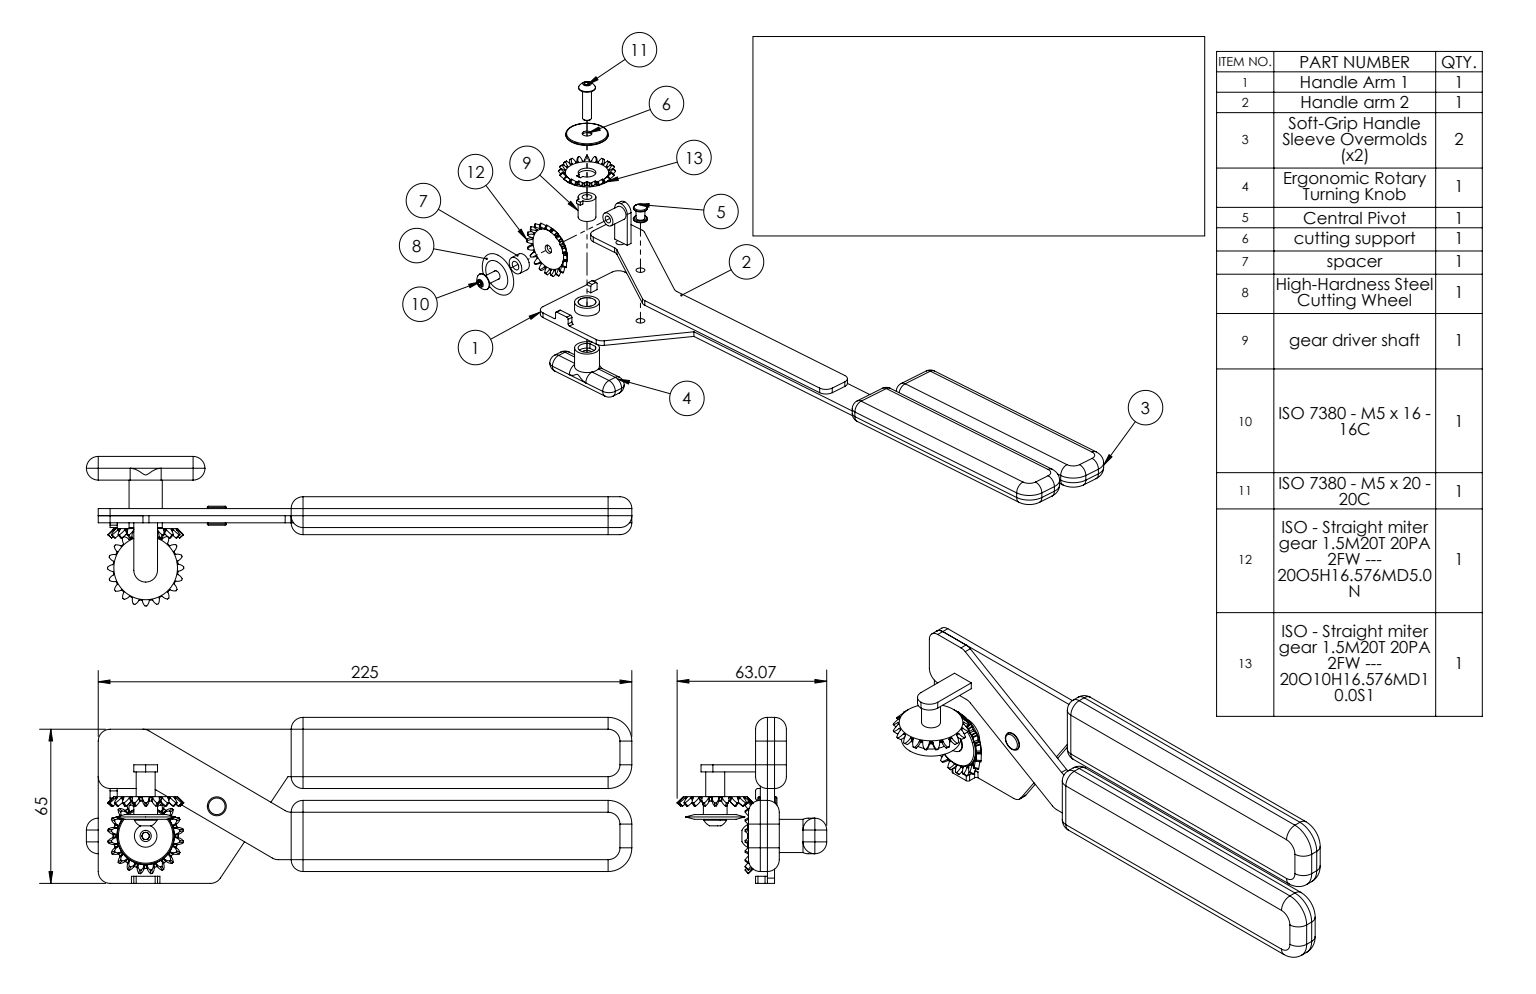
ISO-10303-21;
HEADER;
FILE_DESCRIPTION (('STEP AP214'),
    '1' );
FILE_NAME ('BR-823',
    '2026-09-24T10:15:42',
    ( '' ),
    ( '' ),
    'SwSTEP 2.0',
    'SolidWorks 2026',
    '' );
FILE_SCHEMA (( 'AUTOMOTIVE_DESIGN' ));
ENDSEC;

DATA;
#1 = PRODUCT_DEFINITION_CONTEXT ( 'detailed design', #13776, 'design' ) ;
#2 = DIRECTION ( 'NONE',  ( 0.000000000000000000, 0.000000000000000000, -1.000000000000000000 ) ) ;
#3 = VERTEX_POINT ( 'NONE', #8497 ) ;
#4 = ORIENTED_EDGE ( 'NONE', *, *, #17500, .T. ) ;
#5 = B_SPLINE_CURVE_WITH_KNOTS ( 'NONE', 3,
 ( #7725, #1687, #4752, #9340, #164, #3200, #16319, #9048, #7824, #13639, #557, #15165, #451 ),
 .UNSPECIFIED., .F., .F.,
 ( 4, 3, 3, 3, 4 ),
 ( 1.788933584601082316E-18, 0.0002299804304191483382, 0.0004599608082120253344, 0.0006467586077648016917, 0.0008336169836825988323 ),
 .UNSPECIFIED. ) ;
#6 = CARTESIAN_POINT ( 'NONE',  ( 3.950837973638668288, 0.000000000000000000, 0.000000000000000000 ) ) ;
#8 = ORIENTED_EDGE ( 'NONE', *, *, #17820, .T. ) ;
#7 = CARTESIAN_POINT ( 'NONE',  ( 1.254009781011409919, 5.487405433548389055, 13.61532727684416955 ) ) ;
#9 = CARTESIAN_POINT ( 'NONE',  ( 8.438534575730034959, 3.845978796786118981, -5.688336279099003079 ) ) ;
#10 = DIRECTION ( 'NONE',  ( -0.000000000000000000, 1.000000000000000000, -0.000000000000000000 ) ) ;
#11 = ORIENTED_EDGE ( 'NONE', *, *, #5609, .T. ) ;
#12 = DIRECTION ( 'NONE',  ( -1.000000000000000000, 0.000000000000000000, 0.000000000000000000 ) ) ;
#13 = CARTESIAN_POINT ( 'NONE',  ( 6.538348415311012296, -7.500000000000000888, -12.00000000000000000 ) ) ;
#14 = ORIENTED_EDGE ( 'NONE', *, *, #2662, .F. ) ;
#15 = CARTESIAN_POINT ( 'NONE',  ( 0.3137051932979775248, -0.4596302728638797519, -13.73004976592202553 ) ) ;
#16 =( NAMED_UNIT ( * ) SI_UNIT ( $, .STERADIAN. ) SOLID_ANGLE_UNIT ( ) );
#17 = DIRECTION ( 'NONE',  ( 1.000000000000000000, 0.000000000000000000, 0.000000000000000000 ) ) ;
#18 = CARTESIAN_POINT ( 'NONE',  ( 0.4862570985993235340, -13.89016912371018186, 0.7479633556561964269 ) ) ;
#19 = ADVANCED_FACE ( 'NONE', ( #12879 ), #13081, .T. ) ;
#20 = ADVANCED_FACE ( 'NONE', ( #6722 ), #7157, .F. ) ;
#21 = DIRECTION ( 'NONE',  ( -1.000000000000000000, -0.000000000000000000, -0.000000000000000000 ) ) ;
#22 = CARTESIAN_POINT ( 'NONE',  ( 0.3137051932979775248, 10.83767969834815581, -8.442169467526731808 ) ) ;
#23 =( BOUNDED_SURFACE ( )  B_SPLINE_SURFACE ( 3, 2, ( 
 ( #9096, #13, #15967 ),
 ( #13391, #10337, #14824 ),
 ( #11773, #4513, #14919 ),
 ( #3147, #1737, #16166 ),
 ( #3050, #14723, #10241 ),
 ( #5830, #6041, #1634 ),
 ( #16367, #7585, #7479 ),
 ( #8709, #13293, #11868 ),
 ( #17403, #308, #4405 ),
 ( #11673, #17708, #11585 ),
 ( #4605, #13483, #14634 ),
 ( #10432, #2857, #16066 ),
 ( #10529, #6137, #4319 ),
 ( #1837, #2958, #14535 ),
 ( #11963, #3250, #7675 ),
 ( #1450, #8805, #1543 ),
 ( #7383, #112, #18081 ),
 ( #4980, #16642, #4896 ),
 ( #1935, #13772, #10817 ),
 ( #3545, #6425, #502 ),
 ( #15014, #6332, #12161 ),
 ( #13684, #7870, #13859 ),
 ( #12251, #7768, #685 ),
 ( #777, #6517, #13581 ),
 ( #598, #3730, #9385 ),
 ( #16464, #9186, #5164 ),
 ( #6228, #10723, #12335 ),
 ( #2209, #3349, #8051 ),
 ( #15212, #12061, #18171 ),
 ( #17895, #2122, #17990 ),
 ( #7963, #5070, #3447 ),
 ( #15113, #9558, #10920 ),
 ( #16558, #16740, #4798 ),
 ( #3639, #11009, #16826 ),
 ( #9474, #15389, #9281 ),
 ( #15296, #6610, #2295 ),
 ( #12433, #18262, #8141 ),
 ( #399, #10633, #2029 ),
 ( #867, #11100, #16916 ),
 ( #5524, #4007, #17020 ),
 ( #5350, #5441, #11374 ),
 ( #2657, #12703, #11287 ),
 ( #17193, #15481, #8406 ),
 ( #6984, #18535, #1038 ) ),
 .UNSPECIFIED., .F., .F., .T. ) 
 B_SPLINE_SURFACE_WITH_KNOTS ( ( 4, 2, 2, 2, 2, 2, 2, 2, 2, 2, 2, 2, 2, 2, 2, 2, 2, 2, 2, 2, 2, 4 ),
 ( 3, 3 ),
 ( 0.007984881688765531685, 0.008880023643941203221, 0.009775165599116873022, 0.01067030755429254282, 0.01156544950946821262, 0.01246059146464388243, 0.01335573341981955396, 0.01425087537499522550, 0.01469844635258306040, 0.01492223184137697785, 0.01514601733017089530, 0.01536980281896481275, 0.01559358830775873020, 0.01581737379655264591, 0.01604115928534656510, 0.01693630124052223490, 0.01783144319569790470, 0.01872658515087357797, 0.01962172710604925124, 0.02051686906122492104, 0.02141201101640059085, 0.02230715297157626065 ),
 ( 0.000000000000000000, 1.000000000000000000 ),
 .UNSPECIFIED. ) 
 GEOMETRIC_REPRESENTATION_ITEM ( )  RATIONAL_B_SPLINE_SURFACE ( (
 ( 1.000000000000000000, 0.7071067811865474617, 1.000000000000000000),
 ( 1.000000000000000000, 0.7141735847353027911, 1.000000000000000000),
 ( 1.000000000000000000, 0.7220150969518837059, 1.000000000000000000),
 ( 1.000000000000000000, 0.7390483610380735868, 1.000000000000000000),
 ( 1.000000000000000000, 0.7482852340371979327, 1.000000000000000000),
 ( 1.000000000000000000, 0.7685052920442676516, 1.000000000000000000),
 ( 1.000000000000000000, 0.7795547470752138830, 1.000000000000000000),
 ( 1.000000000000000000, 0.8031735375541008137, 1.000000000000000000),
 ( 1.000000000000000000, 0.8157770400072400507, 1.000000000000000000),
 ( 1.000000000000000000, 0.8424364036431882807, 1.000000000000000000),
 ( 1.000000000000000000, 0.8565278543580017168, 1.000000000000000000),
 ( 1.000000000000000000, 0.8853337094945018526, 1.000000000000000000),
 ( 1.000000000000000000, 0.9000757013528668526, 1.000000000000000000),
 ( 1.000000000000000000, 0.9285356150544983311, 1.000000000000000000),
 ( 1.000000000000000000, 0.9423225300521810288, 1.000000000000000000),
 ( 1.000000000000000000, 0.9592421851076473605, 1.000000000000000000),
 ( 1.000000000000000000, 0.9642414584271679079, 1.000000000000000000),
 ( 1.000000000000000000, 0.9699277023943830844, 1.000000000000000000),
 ( 1.000000000000000000, 0.9715166551480127755, 1.000000000000000000),
 ( 1.000000000000000000, 0.9737696706145027026, 1.000000000000000000),
 ( 1.000000000000000000, 0.9744508395083844032, 1.000000000000000000),
 ( 1.000000000000000000, 0.9748110790397115366, 1.000000000000000000),
 ( 1.000000000000000000, 0.9744748476087098377, 1.000000000000000000),
 ( 1.000000000000000000, 0.9728601655991807595, 1.000000000000000000),
 ( 1.000000000000000000, 0.9715893508620213614, 1.000000000000000000),
 ( 1.000000000000000000, 0.9682746065025299442, 1.000000000000000000),
 ( 1.000000000000000000, 0.9662330922797159882, 1.000000000000000000),
 ( 1.000000000000000000, 0.9616633680012534047, 1.000000000000000000),
 ( 1.000000000000000000, 0.9591230388079813318, 1.000000000000000000),
 ( 1.000000000000000000, 0.9454866025348970249, 1.000000000000000000),
 ( 1.000000000000000000, 0.9317605398179185094, 1.000000000000000000),
 ( 1.000000000000000000, 0.9032287473899394126, 1.000000000000000000),
 ( 1.000000000000000000, 0.8883390392773794497, 1.000000000000000000),
 ( 1.000000000000000000, 0.8592388025803222584, 1.000000000000000000),
 ( 1.000000000000000000, 0.8450030273492604715, 1.000000000000000000),
 ( 1.000000000000000000, 0.8179255325836626289, 1.000000000000000000),
 ( 1.000000000000000000, 0.8050698650503591569, 1.000000000000000000),
 ( 1.000000000000000000, 0.7808988731588855092, 1.000000000000000000),
 ( 1.000000000000000000, 0.7696290231168715357, 1.000000000000000000),
 ( 1.000000000000000000, 0.7490294503509588031, 1.000000000000000000),
 ( 1.000000000000000000, 0.7396188834547082758, 1.000000000000000000),
 ( 1.000000000000000000, 0.7222670797466549386, 1.000000000000000000),
 ( 1.000000000000000000, 0.7142721232192638103, 1.000000000000000000),
 ( 1.000000000000000000, 0.7071067811865517916, 1.000000000000000000) ) ) 
 REPRESENTATION_ITEM ( '' )  SURFACE ( )  );
#24 = FACE_OUTER_BOUND ( 'NONE', #1681, .T. ) ;
#25 = CARTESIAN_POINT ( 'NONE',  ( 0.4862570985993252548, 11.67702470553365401, 7.559321496869467971 ) ) ;
#26 = FACE_BOUND ( 'NONE', #13698, .T. ) ;
#27 = ORIENTED_EDGE ( 'NONE', *, *, #8314, .T. ) ;
#28 = DIRECTION ( 'NONE',  ( 0.000000000000000000, 0.000000000000000000, 1.000000000000000000 ) ) ;
#29 = DIRECTION ( 'NONE',  ( -1.000000000000000000, -0.000000000000000000, -0.000000000000000000 ) ) ;
#30 = ORIENTED_EDGE ( 'NONE', *, *, #17968, .F. ) ;
#31 = VERTEX_POINT ( 'NONE', #18279 ) ;
#33 = CARTESIAN_POINT ( 'NONE',  ( 16.57210152137263393, 0.01136813053532075186, 0.009075239946108242667 ) ) ;
#32 = AXIS2_PLACEMENT_3D ( 'NONE', #18894, #175, #17469 ) ;
#34 = ORIENTED_EDGE ( 'NONE', *, *, #3133, .F. ) ;
#35 = CARTESIAN_POINT ( 'NONE',  ( 0.4862570985993252548, 11.67702470553365401, 7.559321496869467971 ) ) ;
#36 = ORIENTED_EDGE ( 'NONE', *, *, #16394, .F. ) ;
#37 = CARTESIAN_POINT ( 'NONE',  ( 16.56822296793089322, -0.007741272030791128758, 0.006547366384936715959 ) ) ;
#38 = CARTESIAN_POINT ( 'NONE',  ( 0.8740779401507028368, 12.04241618260048696, 7.708543377337672808 ) ) ;
#39 = CARTESIAN_POINT ( 'NONE',  ( -30.00000000000000355, -12.50000000000000178, 6.000000000000000000 ) ) ;
#40 = CARTESIAN_POINT ( 'NONE',  ( 2.747332970342022840, -7.555624153089539163, -14.49942876448600693 ) ) ;
#41 = UNCERTAINTY_MEASURE_WITH_UNIT (LENGTH_MEASURE( 1.000000000000000082E-05 ), #17046, 'distance_accuracy_value', 'NONE');
#42 = PRODUCT_DEFINITION_SHAPE ( 'NONE', 'NONE',  #2847 ) ;
#43 = DIRECTION ( 'NONE',  ( -1.000000000000000000, -0.000000000000000000, -0.000000000000000000 ) ) ;
#44 = DIRECTION ( 'NONE',  ( -0.000000000000000000, 1.000000000000000000, -0.000000000000000000 ) ) ;
#45 =( NAMED_UNIT ( * ) PLANE_ANGLE_UNIT ( ) SI_UNIT ( $, .RADIAN. ) );
#46 = CARTESIAN_POINT ( 'NONE',  ( 3.686287386450715076E-15, -27.00000000000000000, 25.01316734529526187 ) ) ;
#47 = LINE ( 'NONE', #1670, #13971 ) ;
#48 = ADVANCED_FACE ( 'NONE', ( #881 ), #6440, .F. ) ;
#49 = ADVANCED_FACE ( 'NONE', ( #15133 ), #3233, .F. ) ;
#50 = CARTESIAN_POINT ( 'NONE',  ( 16.58200780006414732, 0.01080144354108870768, 0.002844973367391462511 ) ) ;
#51 = CARTESIAN_POINT ( 'NONE',  ( 2.123976203522053297, -14.31368049382965069, -6.261444813538707521 ) ) ;
#52 = EDGE_LOOP ( 'NONE', ( #9471, #1055, #7657, #12818 ) ) ;
#53 = DIRECTION ( 'NONE',  ( 0.000000000000000000, 0.000000000000000000, 1.000000000000000000 ) ) ;
#54 = AXIS2_PLACEMENT_3D ( 'NONE', #4201, #10016, #14696 ) ;
#55 = ORIENTED_EDGE ( 'NONE', *, *, #1230, .F. ) ;
#56 = EDGE_CURVE ( 'NONE', #18903, #4935, #3396, .T. ) ;
#57 = ORIENTED_EDGE ( 'NONE', *, *, #11432, .T. ) ;
#58 = EDGE_LOOP ( 'NONE', ( #12912, #14842, #3064, #3403, #10811, #3564 ) ) ;
#59 = ORIENTED_EDGE ( 'NONE', *, *, #10784, .F. ) ;
#60 = CARTESIAN_POINT ( 'NONE',  ( 1.918921323896324083, -12.08297777410667173, 3.258415356426475729 ) ) ;
#61 = CARTESIAN_POINT ( 'NONE',  ( 1.846138399168762989, -3.446241763653083101, 11.95493567637849530 ) ) ;
#62 =( BOUNDED_SURFACE ( )  B_SPLINE_SURFACE ( 3, 1, ( 
 ( #17504, #8616 ),
 ( #15879, #10145 ),
 ( #4407, #16068 ),
 ( #12913, #2960 ) ),
 .UNSPECIFIED., .F., .F., .T. ) 
 B_SPLINE_SURFACE_WITH_KNOTS ( ( 4, 4 ),
 ( 2, 2 ),
 ( 0.000000000000000000, 1.000000000000000000 ),
 ( 0.000000000000000000, 1.000000000000000000 ),
 .UNSPECIFIED. ) 
 GEOMETRIC_REPRESENTATION_ITEM ( )  RATIONAL_B_SPLINE_SURFACE ( (
 ( 1.000000000000000000, 1.000000000000000000),
 ( 0.9933953342250436691, 0.8357391271907733676),
 ( 0.9933953342250436691, 0.8357391271907733676),
 ( 1.000000000000000000, 1.000000000000000000) ) ) 
 REPRESENTATION_ITEM ( '' )  SURFACE ( )  );
#63 = CARTESIAN_POINT ( 'NONE',  ( 0.3151926232592472954, 8.013596737356548871, -11.16039997398644879 ) ) ;
#64 = ORIENTED_EDGE ( 'NONE', *, *, #16293, .T. ) ;
#65 = CARTESIAN_POINT ( 'NONE',  ( -110.4113270445337918, -81.60345299795268659, -91.28051051278382033 ) ) ;
#66 = LINE ( 'NONE', #18792, #4083 ) ;
#67 = CYLINDRICAL_SURFACE ( 'NONE', #3011, 2.750000000000000000 ) ;
#68 = PRODUCT_RELATED_PRODUCT_CATEGORY ( 'part', '', ( #7466 ) ) ;
#69 = FACE_OUTER_BOUND ( 'NONE', #6354, .T. ) ;
#70 = DIRECTION ( 'NONE',  ( 0.000000000000000000, 0.000000000000000000, 1.000000000000000000 ) ) ;
#71 = EDGE_CURVE ( 'NONE', #14216, #17792, #8218, .T. ) ;
#72 = DIRECTION ( 'NONE',  ( 0.000000000000000000, 0.000000000000000000, -1.000000000000000000 ) ) ;
#73 = CARTESIAN_POINT ( 'NONE',  ( 1.861628059977118888, 9.751736252960505169, 7.751680370224894645 ) ) ;
#74 = EDGE_CURVE ( 'NONE', #18124, #2507, #14609, .T. ) ;
#75 = CARTESIAN_POINT ( 'NONE',  ( 0.3151928476913571364, -11.11539186930580669, -8.075547435847068911 ) ) ;
#76 = ADVANCED_FACE ( 'NONE', ( #2979 ), #15573, .F. ) ;
#77 = CARTESIAN_POINT ( 'NONE',  ( 3.950837973638676281, -6.316429227969562632, 13.10350451991838128 ) ) ;
#78 = VERTEX_POINT ( 'NONE', #4250 ) ;
#79 = B_SPLINE_CURVE_WITH_KNOTS ( 'NONE', 3,
 ( #11643, #13256, #14690, #17565, #11836, #14888, #1601, #176, #17673, #5998, #1801, #7447, #16432 ),
 .UNSPECIFIED., .F., .F.,
 ( 4, 3, 3, 3, 4 ),
 ( 2.453269466693398698E-18, 0.0002299780670421062274, 0.0004599561239687902829, 0.0006896788984287884972, 0.0009194956271626412558 ),
 .UNSPECIFIED. ) ;
#80 = ORIENTED_EDGE ( 'NONE', *, *, #5514, .F. ) ;
#81 = ORIENTED_EDGE ( 'NONE', *, *, #18589, .F. ) ;
#82 = ORIENTED_EDGE ( 'NONE', *, *, #18239, .T. ) ;
#83 = B_SPLINE_CURVE_WITH_KNOTS ( 'NONE', 3,
 ( #3719, #12422, #3534, #6414 ),
 .UNSPECIFIED., .F., .F.,
 ( 4, 4 ),
 ( 2.117499858742978245E-17, 0.003005512676784849197 ),
 .UNSPECIFIED. ) ;
#84 = CARTESIAN_POINT ( 'NONE',  ( 16.56753206892534891, -0.008432171035096417550, 0.004368917149005425125 ) ) ;
#85 = EDGE_CURVE ( 'NONE', #9356, #911, #14003, .T. ) ;
#86 = EDGE_LOOP ( 'NONE', ( #14741, #12706, #5227, #3702 ) ) ;
#87 = DIRECTION ( 'NONE',  ( 0.000000000000000000, 0.000000000000000000, 1.000000000000000000 ) ) ;
#88 = B_SPLINE_CURVE_WITH_KNOTS ( 'NONE', 3,
 ( #11199, #9477, #2212, #17107 ),
 .UNSPECIFIED., .F., .F.,
 ( 4, 4 ),
 ( 2.006682199098010609E-17, 0.003005512676784850064 ),
 .UNSPECIFIED. ) ;
#89 = FACE_OUTER_BOUND ( 'NONE', #1635, .T. ) ;
#90 = DIRECTION ( 'NONE',  ( 0.000000000000000000, 0.000000000000000000, 1.000000000000000000 ) ) ;
#91 = B_SPLINE_CURVE_WITH_KNOTS ( 'NONE', 3,
 ( #3030, #15094, #17687, #2012, #6309, #12042, #7847, #10410, #3227, #4588, #16446, #8878, #7562, #11849, #12235, #14704, #7462, #16246, #1615, #18061, #4965, #7658, #8974, #13373, #10511, #16347, #7751, #17876, #9076, #3330, #14902, #9169, #1913, #12143, #13561, #12586, #2450, #12411 ),
 .UNSPECIFIED., .F., .F.,
 ( 4, 2, 2, 2, 2, 2, 2, 2, 2, 2, 2, 2, 2, 2, 2, 2, 2, 2, 4 ),
 ( 0.000000000000000000, 0.0009058109605214417380, 0.001811621921042883476, 0.002717432881564325105, 0.003623243842085765217, 0.004529054802607205762, 0.005434865763128644139, 0.006340676723650081649, 0.006793582203910802572, 0.007246487684171522628, 0.007699393164432242684, 0.008152298644692964474, 0.009058109605214402851, 0.009963920565735844698, 0.01086973152625728828, 0.01177554248677873013, 0.01268135344730017371, 0.01358716440782161729, 0.01449297536834306087 ),
 .UNSPECIFIED. ) ;
#92 = FACE_BOUND ( 'NONE', #18498, .T. ) ;
#93 = ORIENTED_EDGE ( 'NONE', *, *, #12903, .T. ) ;
#94 = CARTESIAN_POINT ( 'NONE',  ( 0.000000000000000000, 0.000000000000000000, -3.000000000000000000 ) ) ;
#95 = CIRCLE ( 'NONE', #1308, 7.000000000000000000 ) ;
#96 = CARTESIAN_POINT ( 'NONE',  ( 3.664313757352972711, 10.50730552161232545, 9.645155442698788661 ) ) ;
#97 = CARTESIAN_POINT ( 'NONE',  ( -6.538348415311006967, 7.499999999999999112, -17.00000000000000000 ) ) ;
#98 = CARTESIAN_POINT ( 'NONE',  ( 0.3939822652208159193, 8.678192463540325363, -10.75310269629511950 ) ) ;
#99 = CARTESIAN_POINT ( 'NONE',  ( 0.3142011359265332593, 13.17934269988458063, 3.879426116491735854 ) ) ;
#100 = CARTESIAN_POINT ( 'NONE',  ( -6.538348415310934136, -2.500000000000000444, -17.00000000000101252 ) ) ;
#101 = EDGE_LOOP ( 'NONE', ( #9745, #3721, #17119, #3516 ) ) ;
#102 = VERTEX_POINT ( 'NONE', #10357 ) ;
#103 = CARTESIAN_POINT ( 'NONE',  ( 0.000000000000000000, 0.000000000000000000, 0.000000000000000000 ) ) ;
#105 = EDGE_LOOP ( 'NONE', ( #11918, #3838, #18012, #4953 ) ) ;
#104 = CARTESIAN_POINT ( 'NONE',  ( 0.3151928479966097374, 6.943324946344315912E-05, 13.73922861026898623 ) ) ;
#106 = CARTESIAN_POINT ( 'NONE',  ( 0.3170788640506441158, -0.1533108587035203196, -13.74111462631963576 ) ) ;
#107 = AXIS2_PLACEMENT_3D ( 'NONE', #8749, #9037, #10469 ) ;
#108 = CARTESIAN_POINT ( 'NONE',  ( 0.4862570985993235340, -5.003653737315397976, -12.97920246947884770 ) ) ;
#109 = EDGE_CURVE ( 'NONE', #2481, #6541, #2281, .T. ) ;
#110 = ORIENTED_EDGE ( 'NONE', *, *, #15625, .F. ) ;
#111 = CARTESIAN_POINT ( 'NONE',  ( 2.002547531651519996, -11.75462648437105173, 4.532360870844282630 ) ) ;
#112 = CARTESIAN_POINT ( 'NONE',  ( 1.213280723413316275, -7.500000000000199840, -13.07603167631435603 ) ) ;
#113 = ORIENTED_EDGE ( 'NONE', *, *, #10115, .F. ) ;
#114 = CARTESIAN_POINT ( 'NONE',  ( 2.750000000000000000, 0.000000000000000000, 11.00000000000000000 ) ) ;
#115 = DIRECTION ( 'NONE',  ( 0.000000000000000000, 0.000000000000000000, 1.000000000000000000 ) ) ;
#116 = B_SPLINE_CURVE_WITH_KNOTS ( 'NONE', 3,
 ( #18756, #7109, #8540, #9966, #5749, #14281 ),
 .UNSPECIFIED., .F., .F.,
 ( 4, 2, 4 ),
 ( 1.939479807224432123E-18, 0.001657017934710795738, 0.003314035869421589307 ),
 .UNSPECIFIED. ) ;
#117 = CARTESIAN_POINT ( 'NONE',  ( 0.3939875929385652231, -10.75308190953749410, 8.678227324501083473 ) ) ;
#118 = CARTESIAN_POINT ( 'NONE',  ( 2.123976203522053741, 14.31368049382978569, -6.261444813538409981 ) ) ;
#119 = VECTOR ( 'NONE', #9633, 1000.000000000000114 ) ;
#120 = DIRECTION ( 'NONE',  ( -1.000000000000000000, 0.000000000000000000, 0.000000000000000000 ) ) ;
#121 = FACE_OUTER_BOUND ( 'NONE', #17396, .T. ) ;
#122 = FACE_OUTER_BOUND ( 'NONE', #1733, .T. ) ;
#123 = CARTESIAN_POINT ( 'NONE',  ( 0.4754618798421171855, 0.7484603771384397142, 13.89949764182683012 ) ) ;
#124 = CARTESIAN_POINT ( 'NONE',  ( 3.950837973638668288, 14.41405733518061716, 1.958075594453843493 ) ) ;
#125 = ORIENTED_EDGE ( 'NONE', *, *, #5943, .T. ) ;
#126 = CARTESIAN_POINT ( 'NONE',  ( 1.846138399168762989, 4.238866729160403857, 11.69739621335923729 ) ) ;
#127 = CARTESIAN_POINT ( 'NONE',  ( 0.3095370825347224519, -13.20347358821917183, 3.806662003783363613 ) ) ;
#128 = ORIENTED_EDGE ( 'NONE', *, *, #3767, .F. ) ;
#129 = EDGE_CURVE ( 'NONE', #11279, #879, #18664, .T. ) ;
#130 = EDGE_CURVE ( 'NONE', #2733, #15610, #8916, .T. ) ;
#131 = ADVANCED_FACE ( 'NONE', ( #5565 ), #15082, .F. ) ;
#132 = ORIENTED_EDGE ( 'NONE', *, *, #4909, .F. ) ;
#133 = CARTESIAN_POINT ( 'NONE',  ( 0.3170788640506440603, -8.200855617524609897, 11.02668139258439162 ) ) ;
#134 = AXIS2_PLACEMENT_3D ( 'NONE', #17909, #414, #1850 ) ;
#135 = ORIENTED_EDGE ( 'NONE', *, *, #17163, .F. ) ;
#136 = CARTESIAN_POINT ( 'NONE',  ( 2.123976203522053297, 11.67822624909925544, 10.37815841598495936 ) ) ;
#137 = VERTEX_POINT ( 'NONE', #11515 ) ;
#138 = CARTESIAN_POINT ( 'NONE',  ( 0.4862570985993235340, -0.7479633556561480212, -13.89016912371018186 ) ) ;
#139 = CARTESIAN_POINT ( 'NONE',  ( 1.847372867223025406, -7.398914411685061587, 10.00438561114521185 ) ) ;
#140 = CARTESIAN_POINT ( 'NONE',  ( 0.3145729642390374670, 4.535980493005085989, 12.96842777670208768 ) ) ;
#141 = CARTESIAN_POINT ( 'NONE',  ( 0.3150686449036039227, -7.951193823202478583, 11.20479228691394979 ) ) ;
#142 = CARTESIAN_POINT ( 'NONE',  ( 3.377929128793398128, -5.536064832134078628, -12.84367544717941456 ) ) ;
#143 = EDGE_CURVE ( 'NONE', #9064, #209, #1127, .T. ) ;
#144 =( BOUNDED_SURFACE ( )  B_SPLINE_SURFACE ( 3, 1, ( 
 ( #4726, #10659 ),
 ( #8827, #16291 ),
 ( #14654, #136 ),
 ( #10557, #2981 ) ),
 .UNSPECIFIED., .F., .F., .T. ) 
 B_SPLINE_SURFACE_WITH_KNOTS ( ( 4, 4 ),
 ( 2, 2 ),
 ( 0.000000000000000000, 1.000000000000000000 ),
 ( 0.000000000000000000, 1.000000000000000000 ),
 .UNSPECIFIED. ) 
 GEOMETRIC_REPRESENTATION_ITEM ( )  RATIONAL_B_SPLINE_SURFACE ( (
 ( 1.000000000000000000, 1.000000000000000000),
 ( 0.7792777138730160313, 0.9689936506012927220),
 ( 0.7792777138730160313, 0.9689936506012927220),
 ( 1.000000000000000000, 1.000000000000000000) ) ) 
 REPRESENTATION_ITEM ( '' )  SURFACE ( )  );
#145 = AXIS2_PLACEMENT_3D ( 'NONE', #9237, #166, #12114 ) ;
#146 =( NAMED_UNIT ( * ) PLANE_ANGLE_UNIT ( ) SI_UNIT ( $, .RADIAN. ) );
#147 = CARTESIAN_POINT ( 'NONE',  ( 16.57210152137263393, 0.003862718596009277316, 0.01402404281922923004 ) ) ;
#148 = CARTESIAN_POINT ( 'NONE',  ( 16.57605080000000086, 6.123233995736766282E-16, -5.000000000000000000 ) ) ;
#149 = CARTESIAN_POINT ( 'NONE',  ( 16.56872352241294521, -0.001442253899401880124, -0.01033355228142401362 ) ) ;
#150 = VECTOR ( 'NONE', #10844, 1000.000000000000000 ) ;
#151 = CARTESIAN_POINT ( 'NONE',  ( 3.377929128793397684, -9.234024516648242198, -10.50432311212913028 ) ) ;
#152 = B_SPLINE_CURVE_WITH_KNOTS ( 'NONE', 3,
 ( #10208, #11842, #17680, #7551, #14410, #10117 ),
 .UNSPECIFIED., .F., .F.,
 ( 4, 2, 4 ),
 ( 8.940560153363745023E-19, 0.0001828790815881870750, 0.0003657581631763732284 ),
 .UNSPECIFIED. ) ;
#153 = CARTESIAN_POINT ( 'NONE',  ( 1.846524061778021419, -11.93805390544203426, 3.506196582971057740 ) ) ;
#154 = CARTESIAN_POINT ( 'NONE',  ( 16.56753206892534891, -0.004368917149005395635, -0.008432171035096433162 ) ) ;
#155 = ORIENTED_EDGE ( 'NONE', *, *, #10739, .F. ) ;
#156 = ORIENTED_EDGE ( 'NONE', *, *, #8866, .F. ) ;
#157 = ORIENTED_EDGE ( 'NONE', *, *, #6144, .T. ) ;
#158 = ORIENTED_EDGE ( 'NONE', *, *, #3779, .F. ) ;
#159 = CARTESIAN_POINT ( 'NONE',  ( 1.918921323896323639, -9.738309537478938793, -7.860085869556288962 ) ) ;
#160 = EDGE_CURVE ( 'NONE', #16571, #5854, #8950, .T. ) ;
#161 = AXIS2_PLACEMENT_3D ( 'NONE', #1843, #5935, #10343 ) ;
#162 = CARTESIAN_POINT ( 'NONE',  ( 0.000000000000000000, 0.000000000000000000, 3.000000000000000000 ) ) ;
#163 = VECTOR ( 'NONE', #1770, 1000.000000000000227 ) ;
#164 = CARTESIAN_POINT ( 'NONE',  ( 1.847380140988739150, -12.44273713935591097, 0.1101766933248207875 ) ) ;
#165 = ORIENTED_EDGE ( 'NONE', *, *, #2738, .T. ) ;
#166 = DIRECTION ( 'NONE',  ( -0.4246593920385851040, -0.1376957914266804250, 0.8948208031649687033 ) ) ;
#167 = AXIS2_PLACEMENT_3D ( 'NONE', #17284, #15857, #10023 ) ;
#168 = DIRECTION ( 'NONE',  ( 2.775557561562891351E-15, 0.000000000000000000, -1.000000000000000000 ) ) ;
#169 = CARTESIAN_POINT ( 'NONE',  ( 1.846138399168762989, -3.446241763653083101, 11.95493567637849530 ) ) ;
#170 = DIRECTION ( 'NONE',  ( 0.000000000000000000, 0.000000000000000000, 1.000000000000000000 ) ) ;
#171 = CARTESIAN_POINT ( 'NONE',  ( 3.686287386450715076E-15, -16.60000000000000142, 27.11316734529526329 ) ) ;
#172 = ADVANCED_FACE ( 'NONE', ( #1954 ), #15138, .T. ) ;
#173 = DIRECTION ( 'NONE',  ( -0.000000000000000000, -1.000000000000000000, -0.000000000000000000 ) ) ;
#174 = CARTESIAN_POINT ( 'NONE',  ( 8.438534575730034959, -6.862570336891077538, 0.2320579683289888395 ) ) ;
#175 = DIRECTION ( 'NONE',  ( -1.000000000000000000, -0.000000000000000000, -0.000000000000000000 ) ) ;
#176 = CARTESIAN_POINT ( 'NONE',  ( 0.3151926232592474619, -8.137833541809298410, -11.07013665200804198 ) ) ;
#177 = ORIENTED_EDGE ( 'NONE', *, *, #14523, .F. ) ;
#178 =( GEOMETRIC_REPRESENTATION_CONTEXT ( 3 ) GLOBAL_UNCERTAINTY_ASSIGNED_CONTEXT ( ( #14166 ) ) GLOBAL_UNIT_ASSIGNED_CONTEXT ( ( #7797, #12606, #6360 ) ) REPRESENTATION_CONTEXT ( 'NONE', 'WORKASPACE' ) );
#179 = AXIS2_PLACEMENT_3D ( 'NONE', #11361, #10105, #14399 ) ;
#180 = ORIENTED_EDGE ( 'NONE', *, *, #12954, .F. ) ;
#181 = VERTEX_POINT ( 'NONE', #6446 ) ;
#182 = VERTEX_POINT ( 'NONE', #619 ) ;
#183 = ORIENTED_EDGE ( 'NONE', *, *, #15931, .F. ) ;
#184 = CARTESIAN_POINT ( 'NONE',  ( 1.846955891736117517, 11.91257079808168839, 3.593597880662386945 ) ) ;
#185 = CARTESIAN_POINT ( 'NONE',  ( 16.57778382496167424, -0.002851818597093896349, 0.01466529584256787665 ) ) ;
#186 = DIRECTION ( 'NONE',  ( 0.000000000000000000, 0.000000000000000000, -1.000000000000000000 ) ) ;
#187 = EDGE_LOOP ( 'NONE', ( #15081, #15539 ) ) ;
#188 = CARTESIAN_POINT ( 'NONE',  ( 0.3939822652208130327, -0.7002900021918908591, 13.80035637018651862 ) ) ;
#189 = DIRECTION ( 'NONE',  ( -1.000000000000000000, -8.673617379884033500E-16, 0.000000000000000000 ) ) ;
#190 = VECTOR ( 'NONE', #11538, 1000.000000000000000 ) ;
#191 = CARTESIAN_POINT ( 'NONE',  ( 16.56872352241294521, 0.01033355228142401709, -0.001442253899401843694 ) ) ;
#192 = EDGE_CURVE ( 'NONE', #9203, #9252, #8222, .T. ) ;
#193 = LINE ( 'NONE', #2016, #8413 ) ;
#194 = CARTESIAN_POINT ( 'NONE',  ( 25.00000000000000000, 7.499999999999999112, -16.99999999999999645 ) ) ;
#195 = EDGE_CURVE ( 'NONE', #996, #10455, #10657, .T. ) ;
#196 = DIRECTION ( 'NONE',  ( -0.000000000000000000, 1.000000000000000000, -0.000000000000000000 ) ) ;
#197 = ORIENTED_EDGE ( 'NONE', *, *, #8046, .T. ) ;
#198 = LINE ( 'NONE', #14619, #1257 ) ;
#200 = EDGE_LOOP ( 'NONE', ( #4581, #15227, #12383, #13491 ) ) ;
#199 = CARTESIAN_POINT ( 'NONE',  ( 1.847412631396504690, 0.04315047898452520347, -12.44294644888238643 ) ) ;
#201 = CARTESIAN_POINT ( 'NONE',  ( 0.3145734862173252266, 8.321353293018990627, -10.93207848441423913 ) ) ;
#202 = VERTEX_POINT ( 'NONE', #18100 ) ;
#203 = CARTESIAN_POINT ( 'NONE',  ( 0.3170788640506441158, 7.952793437297734691, -11.20690911610894958 ) ) ;
#204 = VERTEX_POINT ( 'NONE', #4724 ) ;
#205 = CARTESIAN_POINT ( 'NONE',  ( 0.000000000000000000, -0.8660254037844384856, -1.500000000000000000 ) ) ;
#206 = PRODUCT ( 'straight miter gear_iso_ISO - Straight miter gear 1.5M20T 20PA 2FW ---20O10H16.576MD10.0S1', 'straight miter gear_iso_ISO - Straight miter gear 1.5M20T 20PA 2FW ---20O10H16.576MD10.0S1', '', ( #2153 ) ) ;
#207 = UNCERTAINTY_MEASURE_WITH_UNIT (LENGTH_MEASURE( 1.000000000000000082E-05 ), #5383, 'distance_accuracy_value', 'NONE');
#208 = PLANE ( 'NONE',  #10210 ) ;
#209 = VERTEX_POINT ( 'NONE', #11985 ) ;
#210 = CARTESIAN_POINT ( 'NONE',  ( 1.847168016377985333, 3.666915430942765397, -11.89018175117590559 ) ) ;
#211 = AXIS2_PLACEMENT_3D ( 'NONE', #14150, #17206, #1054 ) ;
#212 = CARTESIAN_POINT ( 'NONE',  ( 3.950837973638676281, -1.958075594453890789, 14.41405733518059940 ) ) ;
#213 = DIRECTION ( 'NONE',  ( 0.7561779333270775005, 0.1688126975276512953, 0.6322161072786960379 ) ) ;
#214 = AXIS2_PLACEMENT_3D ( 'NONE', #16612, #6578, #9348 ) ;
#215 = ADVANCED_FACE ( 'NONE', ( #233 ), #4532, .T. ) ;
#216 = AXIS2_PLACEMENT_3D ( 'NONE', #4197, #14959, #10013 ) ;
#217 =( GEOMETRIC_REPRESENTATION_CONTEXT ( 3 ) GLOBAL_UNCERTAINTY_ASSIGNED_CONTEXT ( ( #16105 ) ) GLOBAL_UNIT_ASSIGNED_CONTEXT ( ( #3649, #3456, #9291 ) ) REPRESENTATION_CONTEXT ( 'NONE', 'WORKASPACE' ) );
#218 = SURFACE_SIDE_STYLE ('',( #5937 ) ) ;
#220 = VECTOR ( 'NONE', #13485, 1000.000000000000000 ) ;
#219 = CARTESIAN_POINT ( 'NONE',  ( 3.950837973638675393, -2.591948120961912849, 14.31366178983252446 ) ) ;
#221 = EDGE_CURVE ( 'NONE', #1746, #4825, #4915, .T. ) ;
#222 = CARTESIAN_POINT ( 'NONE',  ( -199.9999999999999716, -40.00000000000003553, 0.000000000000000000 ) ) ;
#223 = CARTESIAN_POINT ( 'NONE',  ( 16.56753206892534891, -0.004368917149004301892, 0.008432171035096367243 ) ) ;
#224 = CARTESIAN_POINT ( 'NONE',  ( 3.950837973638675393, -10.05648675950118509, -10.51028938476228980 ) ) ;
#225 = CARTESIAN_POINT ( 'NONE',  ( 3.353306896162455697, -7.069984850384722463, -12.02594772223104869 ) ) ;
#226 = AXIS2_PLACEMENT_3D ( 'NONE', #9917, #9039, #13430 ) ;
#227 = ORIENTED_EDGE ( 'NONE', *, *, #7719, .F. ) ;
#228 = CARTESIAN_POINT ( 'NONE',  ( 2.636624412716062960, 2.862162146982868194, -15.80357026013419564 ) ) ;
#229 = CARTESIAN_POINT ( 'NONE',  ( 0.000000000000000000, 0.000000000000000000, -12.00000000000000000 ) ) ;
#230 = EDGE_LOOP ( 'NONE', ( #7603, #4176, #7702, #11957 ) ) ;
#231 = AXIS2_PLACEMENT_3D ( 'NONE', #2781, #14645, #1752 ) ;
#232 = ORIENTED_EDGE ( 'NONE', *, *, #17218, .F. ) ;
#233 = FACE_OUTER_BOUND ( 'NONE', #2264, .T. ) ;
#234 = ORIENTED_EDGE ( 'NONE', *, *, #6422, .T. ) ;
#235 = CARTESIAN_POINT ( 'NONE',  ( -7.000000000000000000, 0.000000000000000000, 3.000000000000000000 ) ) ;
#236 = ORIENTED_EDGE ( 'NONE', *, *, #1230, .T. ) ;
#237 = FACE_OUTER_BOUND ( 'NONE', #12508, .T. ) ;
#238 = CARTESIAN_POINT ( 'NONE',  ( -114.9284586926032574, -81.60345299795268659, -93.42422730238307338 ) ) ;
#239 = CYLINDRICAL_SURFACE ( 'NONE', #8737, 4.750000000000000000 ) ;
#240 = CARTESIAN_POINT ( 'NONE',  ( 0.3137051932979809665, -13.20008686438108647, 3.805684345189735307 ) ) ;
#241 = VECTOR ( 'NONE', #2260, 1000.000000000000000 ) ;
#242 = CARTESIAN_POINT ( 'NONE',  ( 0.3148208552358926493, -7.888357771040781508, 11.24855514421872726 ) ) ;
#243 = CARTESIAN_POINT ( 'NONE',  ( 1.254255976358384705, 12.44256109021893941, -7.789651112956954115 ) ) ;
#244 =( LENGTH_UNIT ( ) NAMED_UNIT ( * ) SI_UNIT ( .MILLI., .METRE. ) );
#245 = DIRECTION ( 'NONE',  ( 0.000000000000000000, 0.000000000000000000, 1.000000000000000000 ) ) ;
#246 = EDGE_CURVE ( 'NONE', #12932, #11930, #3616, .T. ) ;
#247 = CARTESIAN_POINT ( 'NONE',  ( 2.002547531651519996, 3.242439124566821818, -12.17374746633574745 ) ) ;
#248 = CARTESIAN_POINT ( 'NONE',  ( 2.747332970342022840, 14.49942876448592521, 7.555624153089699924 ) ) ;
#249 = CARTESIAN_POINT ( 'NONE',  ( 0.3137051932979792457, 13.73004976592202198, 0.4596302728640249136 ) ) ;
#250 = B_SPLINE_CURVE_WITH_KNOTS ( 'NONE', 3,
 ( #14214, #9455, #845, #15278, #18327, #2190 ),
 .UNSPECIFIED., .F., .F.,
 ( 4, 2, 4 ),
 ( 2.790109556687801058E-18, 0.0002017457492448093974, 0.0004034914984896159759 ),
 .UNSPECIFIED. ) ;
#251 = CARTESIAN_POINT ( 'NONE',  ( 1.846822687350021974, -11.74004266906801774, -4.121816957446323038 ) ) ;
#252 = CARTESIAN_POINT ( 'NONE',  ( 0.3058872367615226295, -0.6080468242581913429, 13.72992299905059888 ) ) ;
#253 = ORIENTED_EDGE ( 'NONE', *, *, #15488, .F. ) ;
#254 = CIRCLE ( 'NONE', #4224, 11.50000000000000178 ) ;
#255 = ORIENTED_EDGE ( 'NONE', *, *, #85, .F. ) ;
#256 = VERTEX_POINT ( 'NONE', #16289 ) ;
#257 = VERTEX_POINT ( 'NONE', #4999 ) ;
#258 = CARTESIAN_POINT ( 'NONE',  ( 0.3150692679895937820, -7.951395415075003470, -11.20465057551034604 ) ) ;
#259 = CARTESIAN_POINT ( 'NONE',  ( 3.074695600507442172, 6.754521329824937581, 14.01296402267882435 ) ) ;
#260 = CARTESIAN_POINT ( 'NONE',  ( 3.353306896162455697, -12.78841260990234119, -5.573563251762232440 ) ) ;
#261 = AXIS2_PLACEMENT_3D ( 'NONE', #3469, #7605, #6250 ) ;
#262 = ORIENTED_EDGE ( 'NONE', *, *, #15287, .T. ) ;
#263 = LINE ( 'NONE', #16517, #9897 ) ;
#264 = CARTESIAN_POINT ( 'NONE',  ( 2.002547531651519996, -12.57989064830760206, 0.6781519942171299054 ) ) ;
#265 = CARTESIAN_POINT ( 'NONE',  ( 2.636624412714236865, 15.91454522070173638, 2.161493821596668585 ) ) ;
#266 = CARTESIAN_POINT ( 'NONE',  ( 16.56753206892534891, -0.001549402974393209202, 0.009369540855502124857 ) ) ;
#267 = CARTESIAN_POINT ( 'NONE',  ( 0.3150692679895976678, 7.951395415075086959, 11.20465057551027854 ) ) ;
#268 = ADVANCED_FACE ( 'NONE', ( #16665 ), #15218, .F. ) ;
#269 = EDGE_CURVE ( 'NONE', #14945, #13773, #1572, .T. ) ;
#270 = CARTESIAN_POINT ( 'NONE',  ( 2.179449471770337432, -4.500000000000000000, -3.000000000000000000 ) ) ;
#271 = CARTESIAN_POINT ( 'NONE',  ( 2.636624412717099908, 15.80357026013547816, -2.862162146981609201 ) ) ;
#272 = EDGE_CURVE ( 'NONE', #10403, #8116, #15037, .T. ) ;
#273 = CARTESIAN_POINT ( 'NONE',  ( 0.3137051932979757485, -11.37800749014125223, -7.698472063774596030 ) ) ;
#274 = DIRECTION ( 'NONE',  ( 1.000000000000000000, 0.000000000000000000, 0.000000000000000000 ) ) ;
#275 = DIRECTION ( 'NONE',  ( -0.000000000000000000, -0.000000000000000000, -1.000000000000000000 ) ) ;
#276 = ORIENTED_EDGE ( 'NONE', *, *, #18179, .T. ) ;
#277 = B_SPLINE_CURVE_WITH_KNOTS ( 'NONE', 3,
 ( #7928, #18045, #12482, #13739, #10974, #15075 ),
 .UNSPECIFIED., .F., .F.,
 ( 4, 2, 4 ),
 ( 0.000000000000000000, 0.001656992708823638600, 0.003313985417647277200 ),
 .UNSPECIFIED. ) ;
#278 = ORIENTED_EDGE ( 'NONE', *, *, #5786, .T. ) ;
#279 = ORIENTED_EDGE ( 'NONE', *, *, #2294, .T. ) ;
#280 = ORIENTED_EDGE ( 'NONE', *, *, #17255, .F. ) ;
#281 = CARTESIAN_POINT ( 'NONE',  ( 8.522092701127531811, -3.777034505568564349, 5.841710761610117153 ) ) ;
#282 = EDGE_LOOP ( 'NONE', ( #350, #8843, #5301, #9575 ) ) ;
#283 = CARTESIAN_POINT ( 'NONE',  ( 0.4862570985993235340, -11.67702470553359539, -7.559321496869553236 ) ) ;
#284 = CARTESIAN_POINT ( 'NONE',  ( 1.847412631396506022, 11.82061107079964124, 3.886120457021434493 ) ) ;
#285 = CIRCLE ( 'NONE', #10975, 16.06066017081991149 ) ;
#286 = CARTESIAN_POINT ( 'NONE',  ( 2.353870697619109720, 0.7635393531608140050, -12.92712089195301850 ) ) ;
#287 = VERTEX_POINT ( 'NONE', #9120 ) ;
#288 = CARTESIAN_POINT ( 'NONE',  ( 1.846524061778020531, -4.180439405448407975, 11.71897913237548039 ) ) ;
#289 = DIRECTION ( 'NONE',  ( -0.000000000000000000, -0.000000000000000000, 1.000000000000000000 ) ) ;
#290 = CARTESIAN_POINT ( 'NONE',  ( -5.935721797379079234, 7.499999999999999112, -16.97606798286715701 ) ) ;
#291 = FACE_OUTER_BOUND ( 'NONE', #18282, .T. ) ;
#292 = CARTESIAN_POINT ( 'NONE',  ( 2.747332970342022840, 16.17136872824898575, 2.409922051470737348 ) ) ;
#293 = CARTESIAN_POINT ( 'NONE',  ( 0.3150692679895996107, 13.01874238516610482, 4.391039771493711719 ) ) ;
#294 = ADVANCED_FACE ( 'NONE', ( #16576 ), #10453, .T. ) ;
#295 = CARTESIAN_POINT ( 'NONE',  ( 16.56679352167444819, -0.008311568981097361419, 0.004162264567719621902 ) ) ;
#296 = ORIENTED_EDGE ( 'NONE', *, *, #12237, .T. ) ;
#297 = ADVANCED_FACE ( 'NONE', ( #11306 ), #18192, .T. ) ;
#298 = AXIS2_PLACEMENT_3D ( 'NONE', #7660, #11852, #11947 ) ;
#299 = B_SPLINE_CURVE_WITH_KNOTS ( 'NONE', 3,
 ( #4256, #2705, #10076, #18865, #9879, #5572, #15994, #2887, #18769, #12755, #6839, #14374, #14094 ),
 .UNSPECIFIED., .F., .F.,
 ( 4, 3, 3, 3, 4 ),
 ( 2.453269466693398698E-18, 0.0002299804304191474167, 0.0004599608082120242502, 0.0006467586077648022338, 0.0008336169836825977481 ),
 .UNSPECIFIED. ) ;
#300 = DIRECTION ( 'NONE',  ( -0.000000000000000000, 1.000000000000000000, 1.224646799147353207E-16 ) ) ;
#301 = PRESENTATION_LAYER_ASSIGNMENT (  '', '', ( #13725 ) ) ;
#303 = ORIENTED_EDGE ( 'NONE', *, *, #12780, .T. ) ;
#302 = CARTESIAN_POINT ( 'NONE',  ( 1.846822687350021974, 0.2922081769261886675, -12.43915556955403190 ) ) ;
#304 = CARTESIAN_POINT ( 'NONE',  ( 0.3132635586635995617, 11.41586812343490109, 7.641727604903931770 ) ) ;
#305 = CARTESIAN_POINT ( 'NONE',  ( 0.3939822652208148646, -4.930560016699156556, 12.90851734139305229 ) ) ;
#306 = VERTEX_POINT ( 'NONE', #15315 ) ;
#307 = CARTESIAN_POINT ( 'NONE',  ( 0.3170788640506441158, -13.11595226728154984, -4.100430649998100030 ) ) ;
#308 = CARTESIAN_POINT ( 'NONE',  ( 5.084818453916919445, -7.499999999999999112, -13.03762002034291534 ) ) ;
#309 = EDGE_LOOP ( 'NONE', ( #5566, #18701, #10116, #9842 ) ) ;
#310 = CARTESIAN_POINT ( 'NONE',  ( 1.847372867223028070, 3.945260592619209028, -11.80112642014550239 ) ) ;
#311 = CARTESIAN_POINT ( 'NONE',  ( 2.705023505549866147, 7.115606223895331262, -11.23800170568049062 ) ) ;
#312 = CARTESIAN_POINT ( 'NONE',  ( 0.3137051932979792457, -10.83767969834809008, 8.442169467526815296 ) ) ;
#313 = CYLINDRICAL_SURFACE ( 'NONE', #161, 1.000000000000000000 ) ;
#314 = ORIENTED_EDGE ( 'NONE', *, *, #12569, .F. ) ;
#315 = ADVANCED_FACE ( 'NONE', ( #16942 ), #17658, .F. ) ;
#316 = DIRECTION ( 'NONE',  ( -1.000000000000000000, 1.734723475976806848E-16, 0.000000000000000000 ) ) ;
#317 = CARTESIAN_POINT ( 'NONE',  ( 12.00000000000000711, -19.99999999999999645, 8.000000000000000000 ) ) ;
#318 = EDGE_CURVE ( 'NONE', #7741, #3683, #17074, .T. ) ;
#319 = CARTESIAN_POINT ( 'NONE',  ( 16.56872352241294521, -0.004907101719994693724, 0.009207754980063731845 ) ) ;
#320 = DIRECTION ( 'NONE',  ( -0.000000000000000000, 0.000000000000000000, 1.000000000000000000 ) ) ;
#321 = B_SPLINE_CURVE_WITH_KNOTS ( 'NONE', 3,
 ( #17192, #9823, #5805, #5438 ),
 .UNSPECIFIED., .F., .F.,
 ( 4, 4 ),
 ( 0.000000000000000000, 0.002004993803842603211 ),
 .UNSPECIFIED. ) ;
#322 = VERTEX_POINT ( 'NONE', #3941 ) ;
#323 = CARTESIAN_POINT ( 'NONE',  ( 0.3150686449036046444, -4.099563462784746370, 13.11344473514187037 ) ) ;
#324 = CARTESIAN_POINT ( 'NONE',  ( 0.3170788640506440603, 4.100430649997962362, 13.11595226728159425 ) ) ;
#325 = ORIENTED_EDGE ( 'NONE', *, *, #17573, .T. ) ;
#326 = AXIS2_PLACEMENT_3D ( 'NONE', #1638, #13202, #16171 ) ;
#327 = ORIENTED_EDGE ( 'NONE', *, *, #6533, .F. ) ;
#328 = CARTESIAN_POINT ( 'NONE',  ( 0.3145734862173242830, 11.29227530924457312, -7.825584895511399353 ) ) ;
#329 = ORIENTED_EDGE ( 'NONE', *, *, #13463, .T. ) ;
#330 = CARTESIAN_POINT ( 'NONE',  ( 3.950837973638675393, -2.591948120961706792, -14.31366178983255466 ) ) ;
#331 = ORIENTED_EDGE ( 'NONE', *, *, #11334, .T. ) ;
#332 = EDGE_CURVE ( 'NONE', #287, #17311, #2486, .T. ) ;
#333 = DIRECTION ( 'NONE',  ( 0.7635533937278216055, -0.02138673900302784023, 0.6453904417649385383 ) ) ;
#334 = B_SPLINE_CURVE_WITH_KNOTS ( 'NONE', 3,
 ( #18083, #7965, #13393, #210, #17897, #6043, #10532, #310, #6231, #6139, #10434, #16270, #11965 ),
 .UNSPECIFIED., .F., .F.,
 ( 4, 3, 3, 3, 4 ),
 ( 1.734723475976806902E-18, 0.0002299804304191479859, 0.0004599608082120235455, 0.0006467586077647999570, 0.0008336169836825983986 ),
 .UNSPECIFIED. ) ;
#335 = CARTESIAN_POINT ( 'NONE',  ( -54.57590088527786065, 9.999999999999973355, 6.000000000000000000 ) ) ;
#336 = CARTESIAN_POINT ( 'NONE',  ( 0.3148213771069390265, 4.026433757158980775, 13.13560149728601978 ) ) ;
#337 = DIRECTION ( 'NONE',  ( 0.000000000000000000, 0.5000000000000003331, -0.8660254037844383745 ) ) ;
#338 = CARTESIAN_POINT ( 'NONE',  ( 1.560000000000000053, 0.8660254037844389297, -1.500000000000000000 ) ) ;
#339 =( NAMED_UNIT ( * ) SI_UNIT ( $, .STERADIAN. ) SOLID_ANGLE_UNIT ( ) );
#340 = CARTESIAN_POINT ( 'NONE',  ( 1.846955891736119737, 0.2634721419535199782, 12.44001089941741256 ) ) ;
#341 = CARTESIAN_POINT ( 'NONE',  ( 3.950837973638675393, -14.31366178983251380, -2.591948120961955926 ) ) ;
#342 = CARTESIAN_POINT ( 'NONE',  ( 0.4754618798421171855, 5.007009103465246191, 12.98792082933646519 ) ) ;
#343 = FACE_OUTER_BOUND ( 'NONE', #18576, .T. ) ;
#344 = AXIS2_PLACEMENT_3D ( 'NONE', #14911, #300, #1826 ) ;
#345 = CARTESIAN_POINT ( 'NONE',  ( 1.847168016377982669, -11.77471791462001782, 4.022276579849913603 ) ) ;
#346 = CARTESIAN_POINT ( 'NONE',  ( 16.56753206892534891, 0.008432171035096448775, -0.004368917149005361808 ) ) ;
#347 = VERTEX_POINT ( 'NONE', #9760 ) ;
#348 = VERTEX_POINT ( 'NONE', #6727 ) ;
#349 = VERTEX_POINT ( 'NONE', #8162 ) ;
#350 = ORIENTED_EDGE ( 'NONE', *, *, #847, .F. ) ;
#351 = EDGE_CURVE ( 'NONE', #4935, #7190, #5754, .T. ) ;
#352 = CARTESIAN_POINT ( 'NONE',  ( 0.3148208552358962575, 0.2299193288887468323, 13.73693263646118190 ) ) ;
#353 = CARTESIAN_POINT ( 'NONE',  ( 0.3720661004400040439, 10.73619472937714825, -8.694226082900476271 ) ) ;
#354 = CARTESIAN_POINT ( 'NONE',  ( 1.861628059977342264, -3.332996951203546665, -12.00316790821105073 ) ) ;
#355 = DIRECTION ( 'NONE',  ( -0.000000000000000000, 1.000000000000000000, -0.000000000000000000 ) ) ;
#356 = CARTESIAN_POINT ( 'NONE',  ( 0.4862570985993235340, -11.67702470553359539, -7.559321496869553236 ) ) ;
#357 = B_SPLINE_CURVE_WITH_KNOTS ( 'NONE', 3,
 ( #10765, #14764, #7622, #345, #8933, #1676, #3489, #9329, #7716, #7424, #13338, #153, #5976 ),
 .UNSPECIFIED., .F., .F.,
 ( 4, 3, 3, 3, 4 ),
 ( 1.734723475976807094E-18, 0.0002299804304191486635, 0.0004599608082120272860, 0.0006467586077648025591, 0.0008336169836825982902 ),
 .UNSPECIFIED. ) ;
#358 = AXIS2_PLACEMENT_3D ( 'NONE', #13594, #3263, #9294 ) ;
#359 = CARTESIAN_POINT ( 'NONE',  ( 0.4754618798421162973, 0.7484603771386368898, -13.89949764182681768 ) ) ;
#360 = FACE_OUTER_BOUND ( 'NONE', #7164, .T. ) ;
#361 = FACE_OUTER_BOUND ( 'NONE', #4335, .T. ) ;
#362 = CARTESIAN_POINT ( 'NONE',  ( 1.846138399168762101, 11.69739621335927815, -4.238866729160283064 ) ) ;
#363 = CARTESIAN_POINT ( 'NONE',  ( 3.512766787571010241, 14.81029789862133583, -2.682019731918177996 ) ) ;
#364 = CARTESIAN_POINT ( 'NONE',  ( -199.9999999999999716, -10.00000000000002665, 6.000000000000000000 ) ) ;
#365 = DIRECTION ( 'NONE',  ( 1.000000000000000000, 0.000000000000000000, 0.000000000000000000 ) ) ;
#366 = CARTESIAN_POINT ( 'NONE',  ( 0.3148208552358935930, 4.026279359288611026, -13.13564827777585187 ) ) ;
#367 = EDGE_LOOP ( 'NONE', ( #3917, #12671, #3001 ) ) ;
#368 = PRODUCT_DEFINITION_SHAPE ( 'NONE', 'NONE',  #14430 ) ;
#369 = VERTEX_POINT ( 'NONE', #8341 ) ;
#370 = ORIENTED_EDGE ( 'NONE', *, *, #6465, .T. ) ;
#371 = ORIENTED_EDGE ( 'NONE', *, *, #9707, .F. ) ;
#372 = DIRECTION ( 'NONE',  ( 0.000000000000000000, 0.000000000000000000, 1.000000000000000000 ) ) ;
#373 = EDGE_CURVE ( 'NONE', #3822, #11376, #5092, .T. ) ;
#374 = EDGE_CURVE ( 'NONE', #7003, #15103, #2101, .T. ) ;
#375 = EDGE_CURVE ( 'NONE', #5396, #13349, #1164, .T. ) ;
#376 = DIRECTION ( 'NONE',  ( 0.000000000000000000, -0.000000000000000000, 1.000000000000000000 ) ) ;
#377 = CARTESIAN_POINT ( 'NONE',  ( 3.950837973638675393, -13.10350451991835818, -6.316429227969608817 ) ) ;
#378 = CARTESIAN_POINT ( 'NONE',  ( 16.56782317627811096, 0.002708056627497615852, -0.009439921864426480472 ) ) ;
#379 = VECTOR ( 'NONE', #1834, 1000.000000000000227 ) ;
#380 = DIRECTION ( 'NONE',  ( 0.000000000000000000, 0.000000000000000000, -1.000000000000000000 ) ) ;
#381 = VERTEX_POINT ( 'NONE', #5276 ) ;
#382 = CARTESIAN_POINT ( 'NONE',  ( 8.522092701127531811, -4.388629235579537102, -5.397361180353192012 ) ) ;
#383 = CARTESIAN_POINT ( 'NONE',  ( 16.56782317627811096, 0.007739510688079516768, 0.006045301465876390737 ) ) ;
#384 = CARTESIAN_POINT ( 'NONE',  ( 20.00000000000000711, -45.00000000000000000, 6.000000000000000000 ) ) ;
#385 = FACE_OUTER_BOUND ( 'NONE', #17996, .T. ) ;
#386 = CARTESIAN_POINT ( 'NONE',  ( 3.377929128793394575, 5.536064832134161229, 12.84367544717937548 ) ) ;
#387 = PRESENTATION_STYLE_ASSIGNMENT (( #6024 ) ) ;
#388 = EDGE_CURVE ( 'NONE', #11928, #8289, #18271, .T. ) ;
#389 = CARTESIAN_POINT ( 'NONE',  ( 1.918918678667046462, 7.860057224348842020, 9.738328798462404734 ) ) ;
#390 = ORIENTED_EDGE ( 'NONE', *, *, #17273, .T. ) ;
#391 = CARTESIAN_POINT ( 'NONE',  ( 2.636624412714242194, 14.46769361191244485, 6.973567714906650394 ) ) ;
#393 = ORIENTED_EDGE ( 'NONE', *, *, #1315, .T. ) ;
#392 = CARTESIAN_POINT ( 'NONE',  ( 2.636624412714763555, 6.973567714907159321, 14.46769361191226722 ) ) ;
#394 = CARTESIAN_POINT ( 'NONE',  ( 20.00000000000000000, -2.500000000000000444, -17.00000000000000000 ) ) ;
#395 = LINE ( 'NONE', #7672, #17465 ) ;
#396 = MECHANICAL_DESIGN_GEOMETRIC_PRESENTATION_REPRESENTATION (  '', ( #14763 ), #11087 ) ;
#397 = ORIENTED_EDGE ( 'NONE', *, *, #3733, .F. ) ;
#398 = CARTESIAN_POINT ( 'NONE',  ( -59.99999999999997158, -25.00000000000000711, 3.000000000000000000 ) ) ;
#399 = CARTESIAN_POINT ( 'NONE',  ( -6.009712068683241704, -3.596569907853852666, -12.00000000129638345 ) ) ;
#400 = VERTEX_POINT ( 'NONE', #4028 ) ;
#401 = LINE ( 'NONE', #4898, #14257 ) ;
#402 = CARTESIAN_POINT ( 'NONE',  ( 3.074695600507272086, 14.01296402267896291, -6.754521329824639153 ) ) ;
#403 = EDGE_CURVE ( 'NONE', #15002, #6105, #16927, .T. ) ;
#404 = EDGE_CURVE ( 'NONE', #17773, #6765, #13791, .T. ) ;
#405 = CARTESIAN_POINT ( 'NONE',  ( 1.845755665166726844, 11.67596932341234250, 4.296872077620717434 ) ) ;
#406 = CARTESIAN_POINT ( 'NONE',  ( 1.846138399168762989, -4.238866729160486457, 11.69739621335920710 ) ) ;
#407 = ORIENTED_EDGE ( 'NONE', *, *, #468, .F. ) ;
#408 = EDGE_CURVE ( 'NONE', #9965, #18537, #2403, .T. ) ;
#409 = AXIS2_PLACEMENT_3D ( 'NONE', #10692, #1287, #14297 ) ;
#410 =( NAMED_UNIT ( * ) PLANE_ANGLE_UNIT ( ) SI_UNIT ( $, .RADIAN. ) );
#411 = CARTESIAN_POINT ( 'NONE',  ( 3.512766787570708260, -14.91422000116825508, -2.025881399556554552 ) ) ;
#412 = DIRECTION ( 'NONE',  ( 1.000000000000000000, -0.000000000000000000, -0.000000000000000000 ) ) ;
#413 = CARTESIAN_POINT ( 'NONE',  ( 2.636624412717099908, 14.46769361191384817, -6.973567714910368309 ) ) ;
#415 = VERTEX_POINT ( 'NONE', #6635 ) ;
#414 = DIRECTION ( 'NONE',  ( -0.000000000000000000, -0.000000000000000000, 1.000000000000000000 ) ) ;
#416 = CARTESIAN_POINT ( 'NONE',  ( 2.123976203522053297, -11.67822624909917550, -10.37815841598504107 ) ) ;
#417 = ORIENTED_EDGE ( 'NONE', *, *, #14759, .F. ) ;
#418 = CARTESIAN_POINT ( 'NONE',  ( 0.3142014840576498602, -8.382000553815529997, 10.88517824918540278 ) ) ;
#419 = CARTESIAN_POINT ( 'NONE',  ( 1.254255976357772751, -11.25336128106935263, -9.426444230097215993 ) ) ;
#420 = ORIENTED_EDGE ( 'NONE', *, *, #6109, .F. ) ;
#421 = VERTEX_POINT ( 'NONE', #12452 ) ;
#422 = CARTESIAN_POINT ( 'NONE',  ( 3.950837973638677170, 1.958075594453790869, 14.41405733518061538 ) ) ;
#423 = ORIENTED_EDGE ( 'NONE', *, *, #6973, .T. ) ;
#424 = CARTESIAN_POINT ( 'NONE',  ( 1.846138399168762989, 3.446241763652997836, 11.95493567637851839 ) ) ;
#425 = ORIENTED_EDGE ( 'NONE', *, *, #1863, .T. ) ;
#426 = AXIS2_PLACEMENT_3D ( 'NONE', #15769, #12992, #11762 ) ;
#427 = SURFACE_SIDE_STYLE ('',( #3278 ) ) ;
#428 = EDGE_CURVE ( 'NONE', #7816, #11838, #16267, .T. ) ;
#429 = DIRECTION ( 'NONE',  ( 1.000000000000000000, 1.913297951445007868E-16, -0.000000000000000000 ) ) ;
#430 = CARTESIAN_POINT ( 'NONE',  ( 0.3939875929385635023, 13.80036004410494499, -0.7003304234513649806 ) ) ;
#431 = CARTESIAN_POINT ( 'NONE',  ( 16.57210152137263393, 0.01361613799508961699, -0.005118120558001958316 ) ) ;
#432 = CARTESIAN_POINT ( 'NONE',  ( 0.3939822652208138098, 12.90851734139308071, 4.930560016699109482 ) ) ;
#433 = CARTESIAN_POINT ( 'NONE',  ( 16.58200780006414732, -0.009393638146079803797, 0.006043560077721671885 ) ) ;
#434 = EDGE_CURVE ( 'NONE', #181, #4199, #9675, .T. ) ;
#435 = SURFACE_STYLE_USAGE ( .BOTH. , #6368 ) ;
#436 = CARTESIAN_POINT ( 'NONE',  ( 16.58200780006414732, -0.01080144354108868512, -0.002844973367391535370 ) ) ;
#437 = DIRECTION ( 'NONE',  ( -0.000000000000000000, -1.000000000000000000, -0.000000000000000000 ) ) ;
#438 = CARTESIAN_POINT ( 'NONE',  ( 0.3151928476913540278, 8.075884471919755114, 11.11514699826553176 ) ) ;
#439 = CARTESIAN_POINT ( 'NONE',  ( 1.562796894703937678, 6.123233995736766282E-16, -5.000000000000000000 ) ) ;
#440 = EDGE_CURVE ( 'NONE', #202, #1814, #17586, .T. ) ;
#441 = VECTOR ( 'NONE', #16423, 1000.000000000000000 ) ;
#442 = AXIS2_PLACEMENT_3D ( 'NONE', #9810, #18422, #11362 ) ;
#443 = LINE ( 'NONE', #12103, #11221 ) ;
#444 = FACE_OUTER_BOUND ( 'NONE', #3964, .T. ) ;
#445 = ORIENTED_EDGE ( 'NONE', *, *, #10810, .T. ) ;
#446 = ORIENTED_EDGE ( 'NONE', *, *, #4582, .F. ) ;
#447 = VERTEX_POINT ( 'NONE', #5372 ) ;
#448 = ORIENTED_EDGE ( 'NONE', *, *, #10596, .T. ) ;
#449 = CARTESIAN_POINT ( 'NONE',  ( 2.697797270744668019, -3.226410068829341338, -12.89731672021093090 ) ) ;
#450 = CARTESIAN_POINT ( 'NONE',  ( 0.3939822652208129217, -13.80035637018650974, -0.7002900021919380436 ) ) ;
#451 = CARTESIAN_POINT ( 'NONE',  ( 1.846138399168762101, -12.43476674860266229, -0.4167076046096845898 ) ) ;
#452 = CARTESIAN_POINT ( 'NONE',  ( 0.4862570985993235340, -13.44146924561378498, -3.580942890621813923 ) ) ;
#453 = CARTESIAN_POINT ( 'NONE',  ( 5.000000000000000000, 20.00000000000000000, 7.000000000000000000 ) ) ;
#454 = B_SPLINE_CURVE_WITH_KNOTS ( 'NONE', 3,
 ( #13689, #7877, #16649, #3552, #2127, #15217 ),
 .UNSPECIFIED., .F., .F.,
 ( 4, 2, 4 ),
 ( 0.000000000000000000, 0.001656992708822042004, 0.003313985417644083140 ),
 .UNSPECIFIED. ) ;
#455 = PRODUCT_DEFINITION_CONTEXT ( 'detailed design', #9607, 'design' ) ;
#456 = ORIENTED_EDGE ( 'NONE', *, *, #3384, .T. ) ;
#457 = CARTESIAN_POINT ( 'NONE',  ( 3.950837973638675393, -13.10350451991845055, 6.316429227969417859 ) ) ;
#458 = CARTESIAN_POINT ( 'NONE',  ( 2.123976203522053297, 15.54801196254786966, 1.531817366691807125 ) ) ;
#459 = CARTESIAN_POINT ( 'NONE',  ( 2.002547531651519996, -3.242439124566736997, 12.17374746633577232 ) ) ;
#460 = VECTOR ( 'NONE', #9280, 1000.000000000000000 ) ;
#461 = CIRCLE ( 'NONE', #9310, 0.5000000000000004441 ) ;
#462 = EDGE_CURVE ( 'NONE', #17659, #3664, #17402, .T. ) ;
#463 = CARTESIAN_POINT ( 'NONE',  ( 1.846524061778019421, 11.93805390544205913, -3.506196582970981357 ) ) ;
#464 = CARTESIAN_POINT ( 'NONE',  ( 1.918921323896321862, -11.69058285425787247, -4.466082741316331983 ) ) ;
#465 = DIRECTION ( 'NONE',  ( -1.000000000000000000, -0.000000000000000000, -0.000000000000000000 ) ) ;
#466 = AXIS2_PLACEMENT_3D ( 'NONE', #18241, #2269, #18054 ) ;
#467 = DIRECTION ( 'NONE',  ( 1.000000000000000000, 0.000000000000000000, -0.000000000000000000 ) ) ;
#468 = EDGE_CURVE ( 'NONE', #16237, #16692, #17037, .T. ) ;
#469 = ORIENTED_EDGE ( 'NONE', *, *, #3648, .F. ) ;
#470 = ORIENTED_EDGE ( 'NONE', *, *, #8782, .T. ) ;
#471 = VERTEX_POINT ( 'NONE', #14633 ) ;
#472 = AXIS2_PLACEMENT_3D ( 'NONE', #5716, #17109, #4302 ) ;
#473 = VERTEX_POINT ( 'NONE', #7191 ) ;
#474 = AXIS2_PLACEMENT_3D ( 'NONE', #15954, #2942, #11381 ) ;
#475 = CARTESIAN_POINT ( 'NONE',  ( 1.846955891736113298, -7.525208385419886348, -9.909315188408124087 ) ) ;
#476 = CIRCLE ( 'NONE', #16019, 3.499999999999992895 ) ;
#477 = CARTESIAN_POINT ( 'NONE',  ( 16.56782317627811096, 0.003357783021327236019, -0.009228812961909608689 ) ) ;
#478 = DIRECTION ( 'NONE',  ( -1.000000000000000000, -1.298018465182616140E-16, -0.000000000000000000 ) ) ;
#479 = PLANE ( 'NONE',  #15685 ) ;
#480 = DIRECTION ( 'NONE',  ( 0.000000000000000000, 1.000000000000000000, 0.000000000000000000 ) ) ;
#481 = ORIENTED_EDGE ( 'NONE', *, *, #8485, .T. ) ;
#482 = CARTESIAN_POINT ( 'NONE',  ( 1.847412631396500693, -3.886120457021478902, 11.82061107079963413 ) ) ;
#483 = FACE_OUTER_BOUND ( 'NONE', #969, .T. ) ;
#484 = LINE ( 'NONE', #384, #10360 ) ;
#485 = CARTESIAN_POINT ( 'NONE',  ( 16.57778382496167424, -0.01092721432668986720, -0.01018821665058789253 ) ) ;
#486 = DIRECTION ( 'NONE',  ( 0.000000000000000000, 0.000000000000000000, -1.000000000000000000 ) ) ;
#487 = CARTESIAN_POINT ( 'NONE',  ( 0.3151930723728407768, 13.09040889075576608, -4.172946285306434078 ) ) ;
#488 = AXIS2_PLACEMENT_3D ( 'NONE', #18155, #7953, #2196 ) ;
#489 = EDGE_CURVE ( 'NONE', #17676, #8500, #10336, .T. ) ;
#490 = EDGE_CURVE ( 'NONE', #12958, #6376, #11788, .T. ) ;
#491 = EDGE_CURVE ( 'NONE', #2529, #913, #989, .T. ) ;
#492 = VERTEX_POINT ( 'NONE', #16064 ) ;
#493 = DIRECTION ( 'NONE',  ( 0.000000000000000000, 0.000000000000000000, 1.000000000000000000 ) ) ;
#495 = ORIENTED_EDGE ( 'NONE', *, *, #13811, .F. ) ;
#494 = CARTESIAN_POINT ( 'NONE',  ( 3.512766787570729576, 7.127386085303022867, -13.25664064834469613 ) ) ;
#496 = DIRECTION ( 'NONE',  ( 0.000000000000000000, 0.8660254037844384856, 0.5000000000000004441 ) ) ;
#497 = B_SPLINE_CURVE_WITH_KNOTS ( 'NONE', 3,
 ( #14879, #16600, #17753, #3500, #1982, #14773 ),
 .UNSPECIFIED., .F., .F.,
 ( 4, 2, 4 ),
 ( 3.499941646806256644E-17, 0.0001825746017570581273, 0.0003651492035140812891 ),
 .UNSPECIFIED. ) ;
#498 = CARTESIAN_POINT ( 'NONE',  ( 2.320520222536476496, 15.64520721754621491, 1.795797593768047262 ) ) ;
#499 = ORIENTED_EDGE ( 'NONE', *, *, #15873, .T. ) ;
#500 = CARTESIAN_POINT ( 'NONE',  ( 0.3095370825347224519, -13.20347358821911854, -3.806662003783552350 ) ) ;
#501 = CIRCLE ( 'NONE', #2610, 2.499999999999995115 ) ;
#502 = CARTESIAN_POINT ( 'NONE',  ( 0.1927609796801927344, -7.500000000000000888, -14.19253746125320781 ) ) ;
#503 =( GEOMETRIC_REPRESENTATION_CONTEXT ( 3 ) GLOBAL_UNCERTAINTY_ASSIGNED_CONTEXT ( ( #10335 ) ) GLOBAL_UNIT_ASSIGNED_CONTEXT ( ( #244, #6073, #17536 ) ) REPRESENTATION_CONTEXT ( 'NONE', 'WORKASPACE' ) );
#504 = EDGE_LOOP ( 'NONE', ( #8548, #8022, #110, #17428 ) ) ;
#505 = FACE_OUTER_BOUND ( 'NONE', #4433, .T. ) ;
#506 = CARTESIAN_POINT ( 'NONE',  ( 16.57778382496167424, -0.001819584982831791388, -0.01482878558584694619 ) ) ;
#507 = CARTESIAN_POINT ( 'NONE',  ( 1.560000000000000053, 1.299038105676658228, 0.7500000000000009992 ) ) ;
#508 = CARTESIAN_POINT ( 'NONE',  ( 3.074695600507255655, -6.754521329824886955, 14.01296402267885988 ) ) ;
#509 = EDGE_CURVE ( 'NONE', #7915, #137, #6486, .T. ) ;
#510 = EDGE_CURVE ( 'NONE', #16993, #1072, #2856, .T. ) ;
#511 = CARTESIAN_POINT ( 'NONE',  ( 1.918921323896322750, 12.49850046818175286, 0.6349083173280601899 ) ) ;
#512 = ADVANCED_FACE ( 'NONE', ( #8707 ), #17039, .F. ) ;
#513 = EDGE_CURVE ( 'NONE', #10109, #4171, #7612, .T. ) ;
#514 = FACE_OUTER_BOUND ( 'NONE', #15611, .T. ) ;
#516 = ORIENTED_EDGE ( 'NONE', *, *, #14577, .T. ) ;
#515 = PLANE ( 'NONE',  #9065 ) ;
#517 = CARTESIAN_POINT ( 'NONE',  ( 0.3095370825347234511, 10.84046130709058708, 8.444334731364046220 ) ) ;
#518 = ORIENTED_EDGE ( 'NONE', *, *, #5107, .T. ) ;
#519 = CARTESIAN_POINT ( 'NONE',  ( 2.353870697619111052, 12.05847592522643907, 4.720869121224175124 ) ) ;
#520 = CARTESIAN_POINT ( 'NONE',  ( 0.3095370825347234511, -13.20347358821917183, 3.806662003783360504 ) ) ;
#521 = ORIENTED_EDGE ( 'NONE', *, *, #6601, .T. ) ;
#522 = EDGE_LOOP ( 'NONE', ( #4200, #469, #9794, #11121 ) ) ;
#523 = CARTESIAN_POINT ( 'NONE',  ( 8.438534575730034959, 3.845978796786118981, -5.688336279099003079 ) ) ;
#524 = AXIS2_PLACEMENT_3D ( 'NONE', #18729, #5363, #1342 ) ;
#525 = EDGE_LOOP ( 'NONE', ( #13484, #3363, #10680, #18665 ) ) ;
#526 = CARTESIAN_POINT ( 'NONE',  ( 8.438534575730034959, 4.221456476902743837, -5.415535776177475391 ) ) ;
#527 = EDGE_LOOP ( 'NONE', ( #14385, #18414, #1622, #8849 ) ) ;
#528 = AXIS2_PLACEMENT_3D ( 'NONE', #16332, #14594, #1513 ) ;
#529 = CARTESIAN_POINT ( 'NONE',  ( 3.950837973638677170, -14.31366178983255466, 2.591948120961746760 ) ) ;
#530 = VECTOR ( 'NONE', #4094, 1000.000000000000000 ) ;
#531 = LINE ( 'NONE', #14948, #4574 ) ;
#532 = CARTESIAN_POINT ( 'NONE',  ( -33.49999999999999289, -12.50000000000000178, 7.000000000000000000 ) ) ;
#533 = AXIS2_PLACEMENT_3D ( 'NONE', #17391, #8696, #12026 ) ;
#534 = CARTESIAN_POINT ( 'NONE',  ( 0.4862570985993235340, 13.89016912371017476, -0.7479633556562934604 ) ) ;
#535 = CARTESIAN_POINT ( 'NONE',  ( 3.950837973638668288, 0.000000000000000000, 0.000000000000000000 ) ) ;
#536 = AXIS2_PLACEMENT_3D ( 'NONE', #4234, #16950, #9684 ) ;
#537 = PRODUCT ( 'straight miter gear_iso_ISO - Straight miter gear 1.5M20T 20PA 2FW ---20O5H16.576MD5.0N', 'straight miter gear_iso_ISO - Straight miter gear 1.5M20T 20PA 2FW ---20O5H16.576MD5.0N', '', ( #18470 ) ) ;
#538 = CARTESIAN_POINT ( 'NONE',  ( 3.074695600507272086, -2.093687500612061658, 15.41438262616222765 ) ) ;
#539 = DIRECTION ( 'NONE',  ( -0.7635533937278216055, -0.3620487483322522015, 0.5347026451755926280 ) ) ;
#540 =( NAMED_UNIT ( * ) SI_UNIT ( $, .STERADIAN. ) SOLID_ANGLE_UNIT ( ) );
#541 = CARTESIAN_POINT ( 'NONE',  ( 1.846138399168762101, -11.95493567637852905, 3.446241763652952539 ) ) ;
#542 = DIRECTION ( 'NONE',  ( -1.000000000000000000, -0.000000000000000000, -0.000000000000000000 ) ) ;
#543 = VECTOR ( 'NONE', #11601, 1000.000000000000114 ) ;
#544 = AXIS2_PLACEMENT_3D ( 'NONE', #1365, #7303, #320 ) ;
#545 = CARTESIAN_POINT ( 'NONE',  ( 0.4384471787762829753, 8.732395932355681012, 10.76632603192789617 ) ) ;
#546 = EDGE_CURVE ( 'NONE', #1561, #10695, #8743, .T. ) ;
#547 = VECTOR ( 'NONE', #5418, 1000.000000000000000 ) ;
#548 = EDGE_CURVE ( 'NONE', #4649, #6039, #7156, .T. ) ;
#549 = CARTESIAN_POINT ( 'NONE',  ( 1.847034903785825577, -11.76058231742742777, -4.063013886994832013 ) ) ;
#550 = ORIENTED_EDGE ( 'NONE', *, *, #3093, .T. ) ;
#551 = ORIENTED_EDGE ( 'NONE', *, *, #11722, .F. ) ;
#552 = ORIENTED_EDGE ( 'NONE', *, *, #12638, .T. ) ;
#553 = ORIENTED_EDGE ( 'NONE', *, *, #2654, .T. ) ;
#554 =( BOUNDED_SURFACE ( )  B_SPLINE_SURFACE ( 3, 1, ( 
 ( #11504, #4241 ),
 ( #10058, #15887 ),
 ( #10346, #17419 ),
 ( #4328, #14547 ) ),
 .UNSPECIFIED., .F., .F., .T. ) 
 B_SPLINE_SURFACE_WITH_KNOTS ( ( 4, 4 ),
 ( 2, 2 ),
 ( 0.000000000000000000, 1.000000000000000000 ),
 ( 0.000000000000000000, 1.000000000000000000 ),
 .UNSPECIFIED. ) 
 GEOMETRIC_REPRESENTATION_ITEM ( )  RATIONAL_B_SPLINE_SURFACE ( (
 ( 1.000000000000000000, 1.000000000000000000),
 ( 0.7792777138730160313, 0.9689936506012927220),
 ( 0.7792777138730160313, 0.9689936506012927220),
 ( 1.000000000000000000, 1.000000000000000000) ) ) 
 REPRESENTATION_ITEM ( '' )  SURFACE ( )  );
#555 = CARTESIAN_POINT ( 'NONE',  ( 2.636624412714242194, 14.46769361191244485, 6.973567714906650394 ) ) ;
#556 = ADVANCED_BREP_SHAPE_REPRESENTATION ( '', ( #10437, #2030 ), #15178 ) ;
#557 = CARTESIAN_POINT ( 'NONE',  ( 1.846822687350019754, -12.43915556955403545, -0.2922081769261452022 ) ) ;
#558 = DIRECTION ( 'NONE',  ( 0.000000000000000000, -0.000000000000000000, 1.000000000000000000 ) ) ;
#559 = CARTESIAN_POINT ( 'NONE',  ( 0.3939875929385635578, -11.57636969881029110, -7.545068896001335013 ) ) ;
#560 = EDGE_CURVE ( 'NONE', #16555, #5753, #17707, .T. ) ;
#561 = CARTESIAN_POINT ( 'NONE',  ( 1.977436885026408353, 1.488549889122500192, -15.33079650480466860 ) ) ;
#562 = CARTESIAN_POINT ( 'NONE',  ( 1.846822687350018866, -11.92063725419901843, 3.566003975885642774 ) ) ;
#563 = LINE ( 'NONE', #12218, #6284 ) ;
#564 = CARTESIAN_POINT ( 'NONE',  ( 0.3132635586635977853, 12.89236642382228126, -4.743936529203109487 ) ) ;
#565 = DIRECTION ( 'NONE',  ( -0.000000000000000000, 1.000000000000000000, -0.000000000000000000 ) ) ;
#566 = EDGE_CURVE ( 'NONE', #2137, #14073, #11492, .T. ) ;
#567 = EDGE_CURVE ( 'NONE', #18684, #10257, #1633, .T. ) ;
#568 = CARTESIAN_POINT ( 'NONE',  ( 8.522092701127531811, 5.397361180353207111, -4.388629235579518451 ) ) ;
#569 = AXIS2_PLACEMENT_3D ( 'NONE', #9771, #3860, #988 ) ;
#570 = VERTEX_POINT ( 'NONE', #398 ) ;
#571 = ORIENTED_EDGE ( 'NONE', *, *, #13222, .F. ) ;
#572 = EDGE_LOOP ( 'NONE', ( #726, #446 ) ) ;
#573 = EDGE_LOOP ( 'NONE', ( #1318, #5480, #17892, #18760, #5656, #10397, #11984, #9259, #13184, #1949, #6060, #18876, #14646, #9892, #5411 ) ) ;
#574 = B_SPLINE_CURVE_WITH_KNOTS ( 'NONE', 3,
 ( #10643, #11000, #16817, #8132, #6783, #10544 ),
 .UNSPECIFIED., .F., .F.,
 ( 4, 2, 4 ),
 ( 8.673617379884034509E-19, 0.0001828790815886950508, 0.0003657581631773892342 ),
 .UNSPECIFIED. ) ;
#575 = FACE_OUTER_BOUND ( 'NONE', #17278, .T. ) ;
#576 = CARTESIAN_POINT ( 'NONE',  ( 0.000000000000000000, 0.000000000000000000, -3.000000000000000000 ) ) ;
#577 = CARTESIAN_POINT ( 'NONE',  ( 2.749999999999996891, 0.000000000000000000, -6.000000000000000888 ) ) ;
#578 = FACE_BOUND ( 'NONE', #591, .T. ) ;
#579 = ORIENTED_EDGE ( 'NONE', *, *, #14786, .T. ) ;
#580 = CARTESIAN_POINT ( 'NONE',  ( 0.3939875929385661668, 3.598491969338414531, -13.34133634968951831 ) ) ;
#581 = EDGE_CURVE ( 'NONE', #13464, #1391, #8679, .T. ) ;
#582 = CARTESIAN_POINT ( 'NONE',  ( -20.00000000000000000, 2.499999999999998668, -16.99999999999999645 ) ) ;
#583 = CARTESIAN_POINT ( 'NONE',  ( -5.052632128771760378, 7.499999999999999112, -16.81774875490144083 ) ) ;
#584 = CARTESIAN_POINT ( 'NONE',  ( 1.846138399168762989, 11.69739621335922308, 4.238866729160444713 ) ) ;
#585 = DIRECTION ( 'NONE',  ( -0.000000000000000000, -0.000000000000000000, -1.000000000000000000 ) ) ;
#586 = EDGE_CURVE ( 'NONE', #8358, #2858, #15012, .T. ) ;
#587 = CARTESIAN_POINT ( 'NONE',  ( 16.57210152137263393, -0.008007331252333342933, 0.01214401161737632510 ) ) ;
#588 = CARTESIAN_POINT ( 'NONE',  ( 2.320520222538862143, 13.71278186123479870, -7.743191299716691844 ) ) ;
#589 =( BOUNDED_SURFACE ( )  B_SPLINE_SURFACE ( 3, 1, ( 
 ( #17899, #13586 ),
 ( #9192, #12166 ),
 ( #14923, #3353 ),
 ( #1842, #1548 ) ),
 .UNSPECIFIED., .F., .F., .T. ) 
 B_SPLINE_SURFACE_WITH_KNOTS ( ( 4, 4 ),
 ( 2, 2 ),
 ( 0.000000000000000000, 1.000000000000000000 ),
 ( 0.000000000000000000, 1.000000000000000000 ),
 .UNSPECIFIED. ) 
 GEOMETRIC_REPRESENTATION_ITEM ( )  RATIONAL_B_SPLINE_SURFACE ( (
 ( 1.000000000000000000, 1.000000000000000000),
 ( 0.9593108457356467333, 0.9995965569486454649),
 ( 0.9593108457356467333, 0.9995965569486454649),
 ( 1.000000000000000000, 1.000000000000000000) ) ) 
 REPRESENTATION_ITEM ( '' )  SURFACE ( )  );
#590 =( BOUNDED_SURFACE ( )  B_SPLINE_SURFACE ( 3, 1, ( 
 ( #16855, #18019 ),
 ( #6645, #6547 ),
 ( #10853, #18107 ),
 ( #1964, #8079 ) ),
 .UNSPECIFIED., .F., .F., .T. ) 
 B_SPLINE_SURFACE_WITH_KNOTS ( ( 4, 4 ),
 ( 2, 2 ),
 ( 0.000000000000000000, 1.000000000000000000 ),
 ( 0.000000000000000000, 1.000000000000000000 ),
 .UNSPECIFIED. ) 
 GEOMETRIC_REPRESENTATION_ITEM ( )  RATIONAL_B_SPLINE_SURFACE ( (
 ( 1.000000000000000000, 1.000000000000000000),
 ( 0.7792777138730158093, 0.9689936506012928330),
 ( 0.7792777138730158093, 0.9689936506012928330),
 ( 1.000000000000000000, 1.000000000000000000) ) ) 
 REPRESENTATION_ITEM ( '' )  SURFACE ( )  );
#591 = EDGE_LOOP ( 'NONE', ( #390, #2249 ) ) ;
#592 = DIRECTION ( 'NONE',  ( 1.000000000000000000, 0.000000000000000000, 0.000000000000000000 ) ) ;
#594 = EDGE_LOOP ( 'NONE', ( #10018, #5497, #2207, #4575 ) ) ;
#593 = CARTESIAN_POINT ( 'NONE',  ( 2.636624412716902288, 7.605649742760546950, -14.14563173255513995 ) ) ;
#595 = CARTESIAN_POINT ( 'NONE',  ( 1.846138399168762101, 11.69739621335927815, -4.238866729160283064 ) ) ;
#596 = ORIENTED_EDGE ( 'NONE', *, *, #12490, .T. ) ;
#597 = CARTESIAN_POINT ( 'NONE',  ( 0.3170788640506440603, -13.02120094575825249, -4.392045232375947350 ) ) ;
#598 = CARTESIAN_POINT ( 'NONE',  ( -0.9371186270710654131, -6.939831204821797606, -11.99999999628260916 ) ) ;
#599 = EDGE_LOOP ( 'NONE', ( #4795, #7309, #27, #8867 ) ) ;
#600 = CARTESIAN_POINT ( 'NONE',  ( 16.56679352167444819, -0.009190982326619374226, 0.001390132774595425865 ) ) ;
#601 = ADVANCED_FACE ( 'NONE', ( #10334 ), #6040, .F. ) ;
#602 = CARTESIAN_POINT ( 'NONE',  ( 0.4862570985993235340, 12.97920246947886191, -5.003653737315353567 ) ) ;
#603 = DIRECTION ( 'NONE',  ( -0.5000000000000042188, 0.000000000000000000, 0.8660254037844361541 ) ) ;
#604 = EDGE_LOOP ( 'NONE', ( #14793, #13660, #11416, #15705, #8901, #5633, #7673, #18303, #12840, #5256, #1516, #16722, #14127, #4359, #12811, #8779, #820, #15702, #13342, #11139, #18510, #3613, #16269, #17169, #11483, #6561, #9871, #1346, #1933, #13849, #5209, #16099, #11607, #15015, #64, #7840, #14789, #5799, #11534, #1904, #788, #234, #2284, #5679, #3871, #5268, #7358, #7934, #11240, #1415, #14792, #9803, #10433, #12173, #14090, #8455, #17629, #14404, #16264, #8778, #14227, #17453, #4483, #11461 ) ) ;
#605 = CIRCLE ( 'NONE', #298, 5.000000000000000888 ) ;
#606 = CIRCLE ( 'NONE', #10991, 0.5000000000000004441 ) ;
#607 =( LENGTH_UNIT ( ) NAMED_UNIT ( * ) SI_UNIT ( .MILLI., .METRE. ) );
#608 = CARTESIAN_POINT ( 'NONE',  ( 3.074695600507147297, -15.41438262616236088, -2.093687500612132268 ) ) ;
#609 = CARTESIAN_POINT ( 'NONE',  ( 1.560000000000000053, 0.8660254037844389297, -1.500000000000000000 ) ) ;
#611 = ORIENTED_EDGE ( 'NONE', *, *, #1777, .T. ) ;
#610 = CARTESIAN_POINT ( 'NONE',  ( 0.4385251269669946939, -11.63205320541528209, 7.540955776459703053 ) ) ;
#612 = CARTESIAN_POINT ( 'NONE',  ( 16.56872352241294521, -0.01027347319884440620, 0.001821578298044753286 ) ) ;
#613 = CIRCLE ( 'NONE', #11582, 5.000000000000000000 ) ;
#614 = CARTESIAN_POINT ( 'NONE',  ( 16.56753206892534891, 0.001549402974394159613, 0.009369540855502535986 ) ) ;
#615 = CARTESIAN_POINT ( 'NONE',  ( 14.99999999999999289, 20.00000000000000000, 3.000000000000000000 ) ) ;
#616 = CARTESIAN_POINT ( 'NONE',  ( 8.438534575730034959, 1.899950616255281055, -6.598402093327859319 ) ) ;
#617 = VERTEX_POINT ( 'NONE', #10631 ) ;
#618 = VERTEX_POINT ( 'NONE', #13291 ) ;
#619 = CARTESIAN_POINT ( 'NONE',  ( 15.00000000000000711, -45.00000000000000000, 6.000000000000000000 ) ) ;
#620 = VERTEX_POINT ( 'NONE', #1836 ) ;
#621 = DIRECTION ( 'NONE',  ( 0.7635533937278214944, -0.3966532189476670300, 0.5095610256143814354 ) ) ;
#622 = VERTEX_POINT ( 'NONE', #3146 ) ;
#623 = EDGE_CURVE ( 'NONE', #15645, #13108, #16050, .T. ) ;
#624 = ADVANCED_FACE ( 'NONE', ( #14823 ), #6227, .F. ) ;
#625 = EDGE_CURVE ( 'NONE', #6956, #6611, #15112, .T. ) ;
#626 = FILL_AREA_STYLE ('',( #13710 ) ) ;
#627 = CARTESIAN_POINT ( 'NONE',  ( 2.747332970342022840, -14.49942876448586482, -7.555624153089806505 ) ) ;
#628 = CARTESIAN_POINT ( 'NONE',  ( 0.3137051932979792457, -3.805684345189695783, -13.20008686438109891 ) ) ;
#629 = CARTESIAN_POINT ( 'NONE',  ( 3.074695600507183268, 7.366518011946177502, -13.70113613813200537 ) ) ;
#630 = LINE ( 'NONE', #13714, #10563 ) ;
#631 = FACE_OUTER_BOUND ( 'NONE', #11718, .T. ) ;
#632 = DIRECTION ( 'NONE',  ( 0.000000000000000000, 0.000000000000000000, -1.000000000000000000 ) ) ;
#633 = CARTESIAN_POINT ( 'NONE',  ( 0.4862570985993235340, 3.580942890621860109, -13.44146924561377254 ) ) ;
#634 = CARTESIAN_POINT ( 'NONE',  ( 0.3939875929385670550, -12.90850834464103691, 4.930599594904505167 ) ) ;
#635 = LINE ( 'NONE', #5205, #2069 ) ;
#636 = EDGE_LOOP ( 'NONE', ( #8757, #7356, #11328, #12997 ) ) ;
#637 = ORIENTED_EDGE ( 'NONE', *, *, #9764, .F. ) ;
#638 = ORIENTED_EDGE ( 'NONE', *, *, #5134, .T. ) ;
#639 = ORIENTED_EDGE ( 'NONE', *, *, #11001, .F. ) ;
#640 = ORIENTED_EDGE ( 'NONE', *, *, #8910, .T. ) ;
#641 = ORIENTED_EDGE ( 'NONE', *, *, #13469, .F. ) ;
#642 = CARTESIAN_POINT ( 'NONE',  ( -108.0624185875376639, -81.60345299795268659, -90.16577778219220818 ) ) ;
#643 = CARTESIAN_POINT ( 'NONE',  ( -20.00000000000000000, 2.499999999999998668, -16.99999999999999645 ) ) ;
#644 = CARTESIAN_POINT ( 'NONE',  ( 1.845756295923353996, 9.776763338604718356, -7.694561132136850112 ) ) ;
#645 = EDGE_CURVE ( 'NONE', #12951, #4745, #12694, .T. ) ;
#646 = CARTESIAN_POINT ( 'NONE',  ( 8.522092701127531811, -2.505958102592576342, -6.489356537178215589 ) ) ;
#647 = CARTESIAN_POINT ( 'NONE',  ( 15.00000000000000711, -19.99999999999999645, 6.000000000000000000 ) ) ;
#648 = EDGE_CURVE ( 'NONE', #1182, #5121, #7868, .T. ) ;
#649 = CARTESIAN_POINT ( 'NONE',  ( 16.56872352241294521, -0.01027347319884365333, -0.001821578298043897851 ) ) ;
#650 = CARTESIAN_POINT ( 'NONE',  ( 0.000000000000000000, 0.000000000000000000, 10.49999999999999822 ) ) ;
#651 = DIRECTION ( 'NONE',  ( 0.000000000000000000, 0.000000000000000000, 1.000000000000000000 ) ) ;
#652 = CARTESIAN_POINT ( 'NONE',  ( 3.664313757352978485, 12.42002390572636372, -7.012524439851359759 ) ) ;
#653 = ADVANCED_FACE ( 'NONE', ( #7584 ), #14245, .F. ) ;
#654 = ORIENTED_EDGE ( 'NONE', *, *, #12850, .T. ) ;
#655 =( BOUNDED_SURFACE ( )  B_SPLINE_SURFACE ( 3, 1, ( 
 ( #1723, #9084 ),
 ( #18316, #14908 ),
 ( #7574, #5133 ),
 ( #14014, #8108 ) ),
 .UNSPECIFIED., .F., .F., .T. ) 
 B_SPLINE_SURFACE_WITH_KNOTS ( ( 4, 4 ),
 ( 2, 2 ),
 ( 0.000000000000000000, 1.000000000000000000 ),
 ( 0.000000000000000000, 1.000000000000000000 ),
 .UNSPECIFIED. ) 
 GEOMETRIC_REPRESENTATION_ITEM ( )  RATIONAL_B_SPLINE_SURFACE ( (
 ( 1.000000000000000000, 1.000000000000000000),
 ( 0.9593108457356467333, 0.9995965569486454649),
 ( 0.9593108457356467333, 0.9995965569486454649),
 ( 1.000000000000000000, 1.000000000000000000) ) ) 
 REPRESENTATION_ITEM ( '' )  SURFACE ( )  );
#656 = ORIENTED_EDGE ( 'NONE', *, *, #2270, .T. ) ;
#657 = ORIENTED_EDGE ( 'NONE', *, *, #5467, .T. ) ;
#658 = ORIENTED_EDGE ( 'NONE', *, *, #9985, .F. ) ;
#659 = DIRECTION ( 'NONE',  ( 0.000000000000000000, 1.000000000000000000, 0.000000000000000000 ) ) ;
#660 = CARTESIAN_POINT ( 'NONE',  ( 3.353306896162455697, -1.348936822032921423, 13.88482890973696016 ) ) ;
#661 = VECTOR ( 'NONE', #6476, 1000.000000000000000 ) ;
#662 = CARTESIAN_POINT ( 'NONE',  ( 1.847247051441588184, -7.177495230324629105, -10.16425585218608951 ) ) ;
#663 = CARTESIAN_POINT ( 'NONE',  ( 3.664313757352974932, -5.926151963190458893, 12.97355833021538096 ) ) ;
#664 = EDGE_CURVE ( 'NONE', #10558, #9813, #10583, .T. ) ;
#665 = CARTESIAN_POINT ( 'NONE',  ( 18.75000000000000000, 2.789133085058096608E-16, -2.055000000000000160 ) ) ;
#666 = VERTEX_POINT ( 'NONE', #13954 ) ;
#667 = CARTESIAN_POINT ( 'NONE',  ( 2.002547531651519996, -0.6781519942172617998, 12.57989064830759318 ) ) ;
#668 = CARTESIAN_POINT ( 'NONE',  ( 1.847034903785825577, -11.76058231742742777, -4.063013886994832013 ) ) ;
#669 = EDGE_CURVE ( 'NONE', #1858, #9927, #12604, .T. ) ;
#670 = ADVANCED_FACE ( 'NONE', ( #3543 ), #3340, .T. ) ;
#671 = CARTESIAN_POINT ( 'NONE',  ( -4.545271119322114473, 5.336083332029744497, -11.99999999554324681 ) ) ;
#672 = LINE ( 'NONE', #13468, #4172 ) ;
#673 = DIRECTION ( 'NONE',  ( 1.000000000000000000, 0.000000000000000000, -0.000000000000000000 ) ) ;
#674 = CARTESIAN_POINT ( 'NONE',  ( 2.636624412714236865, 0.000000000000000000, 0.000000000000000000 ) ) ;
#675 = CARTESIAN_POINT ( 'NONE',  ( 0.3137051932979809665, 13.20008686438111312, -3.805684345189650042 ) ) ;
#676 = ORIENTED_EDGE ( 'NONE', *, *, #4525, .T. ) ;
#678 = VERTEX_POINT ( 'NONE', #5254 ) ;
#677 = CARTESIAN_POINT ( 'NONE',  ( 8.438534575730034959, -4.221456476902702981, 5.415535776177505589 ) ) ;
#679 = CARTESIAN_POINT ( 'NONE',  ( 2.705023505549862595, -13.27418276223636795, 0.8488853074252508124 ) ) ;
#680 = EDGE_CURVE ( 'NONE', #4361, #18405, #6716, .T. ) ;
#681 = AXIS2_PLACEMENT_3D ( 'NONE', #16263, #10, #9092 ) ;
#682 = EDGE_LOOP ( 'NONE', ( #16738, #16669, #5316, #11820 ) ) ;
#683 = CARTESIAN_POINT ( 'NONE',  ( 1.847372867223029846, -3.744745203533896394, -11.86627781945711924 ) ) ;
#684 = PRODUCT ( 'Ergonomic Rotary Turning Knob', 'Ergonomic Rotary Turning Knob', '', ( #12370 ) ) ;
#685 = CARTESIAN_POINT ( 'NONE',  ( -0.1127451301830492136, -7.500000000000000888, -14.18240585847551571 ) ) ;
#686 = EDGE_LOOP ( 'NONE', ( #13746, #6468, #7548, #2921 ) ) ;
#687 = CARTESIAN_POINT ( 'NONE',  ( 2.353870697619111496, 8.216087327473076130, -10.00946331859655203 ) ) ;
#688 = CARTESIAN_POINT ( 'NONE',  ( 2.636624412717099908, 14.46769361191384817, -6.973567714910368309 ) ) ;
#689 = CARTESIAN_POINT ( 'NONE',  ( 1.959212340397945562, -11.71715421693495074, -4.509090217468642692 ) ) ;
#690 =( BOUNDED_SURFACE ( )  B_SPLINE_SURFACE ( 3, 1, ( 
 ( #16837, #9567 ),
 ( #4019, #966 ),
 ( #12441, #17029 ),
 ( #12716, #12808 ) ),
 .UNSPECIFIED., .F., .F., .T. ) 
 B_SPLINE_SURFACE_WITH_KNOTS ( ( 4, 4 ),
 ( 2, 2 ),
 ( 0.000000000000000000, 1.000000000000000000 ),
 ( 0.000000000000000000, 1.000000000000000000 ),
 .UNSPECIFIED. ) 
 GEOMETRIC_REPRESENTATION_ITEM ( )  RATIONAL_B_SPLINE_SURFACE ( (
 ( 1.000000000000000000, 1.000000000000000000),
 ( 0.7792777138730158093, 0.9689936506012928330),
 ( 0.7792777138730158093, 0.9689936506012928330),
 ( 1.000000000000000000, 1.000000000000000000) ) ) 
 REPRESENTATION_ITEM ( '' )  SURFACE ( )  );
#691 =( BOUNDED_SURFACE ( )  B_SPLINE_SURFACE ( 3, 1, ( 
 ( #14444, #5933 ),
 ( #10146, #4516 ),
 ( #11496, #11777 ),
 ( #17606, #1351 ) ),
 .UNSPECIFIED., .F., .F., .T. ) 
 B_SPLINE_SURFACE_WITH_KNOTS ( ( 4, 4 ),
 ( 2, 2 ),
 ( 0.000000000000000000, 1.000000000000000000 ),
 ( 0.000000000000000000, 1.000000000000000000 ),
 .UNSPECIFIED. ) 
 GEOMETRIC_REPRESENTATION_ITEM ( )  RATIONAL_B_SPLINE_SURFACE ( (
 ( 1.000000000000000000, 1.000000000000000000),
 ( 0.7792777138730160313, 0.9689936506012927220),
 ( 0.7792777138730160313, 0.9689936506012927220),
 ( 1.000000000000000000, 1.000000000000000000) ) ) 
 REPRESENTATION_ITEM ( '' )  SURFACE ( )  );
#692 = CARTESIAN_POINT ( 'NONE',  ( 15.00000000000000711, -19.99999999999999645, 8.000000000000000000 ) ) ;
#693 = VECTOR ( 'NONE', #8023, 1000.000000000000000 ) ;
#694 =( NAMED_UNIT ( * ) SI_UNIT ( $, .STERADIAN. ) SOLID_ANGLE_UNIT ( ) );
#695 = EDGE_CURVE ( 'NONE', #306, #15917, #9432, .T. ) ;
#696 = CARTESIAN_POINT ( 'NONE',  ( 1.847034903785822468, -10.19974412751570014, 7.126331315909236075 ) ) ;
#698 = VERTEX_POINT ( 'NONE', #9649 ) ;
#697 = CARTESIAN_POINT ( 'NONE',  ( 16.56782317627811096, -0.005492611183757366636, 0.008141063682853383679 ) ) ;
#699 = CARTESIAN_POINT ( 'NONE',  ( 3.377929128793395019, 9.234024516648318581, 10.50432311212905923 ) ) ;
#700 = EDGE_CURVE ( 'NONE', #6674, #10089, #4653, .T. ) ;
#701 = DIRECTION ( 'NONE',  ( -1.000000000000000000, -0.000000000000000000, -0.000000000000000000 ) ) ;
#702 = DIRECTION ( 'NONE',  ( 0.000000000000000000, 0.000000000000000000, 1.000000000000000000 ) ) ;
#703 = CARTESIAN_POINT ( 'NONE',  ( 1.977436885026283564, -11.52792723756319582, -10.21547824869606202 ) ) ;
#704 = ORIENTED_EDGE ( 'NONE', *, *, #13489, .F. ) ;
#705 = ORIENTED_EDGE ( 'NONE', *, *, #17842, .F. ) ;
#706 = DIRECTION ( 'NONE',  ( 0.7561779333270775005, -0.6534392409364819798, -0.03481510524965015368 ) ) ;
#707 = CARTESIAN_POINT ( 'NONE',  ( -33.99999999999999289, -12.50000000000000178, -0.5000000000000000000 ) ) ;
#708 = ORIENTED_EDGE ( 'NONE', *, *, #6862, .T. ) ;
#709 = CYLINDRICAL_SURFACE ( 'NONE', #9338, 5.000000000000000000 ) ;
#710 = CARTESIAN_POINT ( 'NONE',  ( -199.9999999999999716, -5.000000000000024869, 3.000000000000000000 ) ) ;
#711 = PLANE ( 'NONE',  #11015 ) ;
#712 = CARTESIAN_POINT ( 'NONE',  ( 8.522092701127531811, 4.388629235579655230, -5.397361180353095200 ) ) ;
#713 = CARTESIAN_POINT ( 'NONE',  ( 0.4862570985993235340, 13.44146924561385958, -3.580942890621532371 ) ) ;
#714 = CIRCLE ( 'NONE', #15639, 14.54644660717763927 ) ;
#715 = B_SPLINE_CURVE_WITH_KNOTS ( 'NONE', 3,
 ( #8013, #2176, #9524, #5223 ),
 .UNSPECIFIED., .F., .F.,
 ( 4, 4 ),
 ( 2.076240083260000355E-17, 0.003005512676784849197 ),
 .UNSPECIFIED. ) ;
#716 = SURFACE_STYLE_FILL_AREA ( #10759 ) ;
#717 = DIRECTION ( 'NONE',  ( -0.7561779333270775005, 0.5081796452863305280, -0.4122479608995649469 ) ) ;
#718 = CARTESIAN_POINT ( 'NONE',  ( 3.950837973638676281, 6.316429227969464932, 13.10350451991842569 ) ) ;
#719 = CARTESIAN_POINT ( 'NONE',  ( 0.3307726912345230752, 3.680742887039495148, -13.25328329128662119 ) ) ;
#720 = CARTESIAN_POINT ( 'NONE',  ( -61.35602477868047799, -10.00000000000000888, 6.000000000000000000 ) ) ;
#721 = EDGE_CURVE ( 'NONE', #17138, #1603, #13761, .T. ) ;
#722 = EDGE_CURVE ( 'NONE', #14617, #1651, #2384, .T. ) ;
#723 = EDGE_CURVE ( 'NONE', #14183, #11279, #13412, .T. ) ;
#724 = FACE_BOUND ( 'NONE', #4955, .T. ) ;
#725 = CARTESIAN_POINT ( 'NONE',  ( 0.4862570985993235340, -7.559321496869506163, 11.67702470553362559 ) ) ;
#726 = ORIENTED_EDGE ( 'NONE', *, *, #6443, .F. ) ;
#727 = AXIS2_PLACEMENT_3D ( 'NONE', #3087, #13233, #10571 ) ;
#728 = TOROIDAL_SURFACE ( 'NONE', #7132, 11.50000000000000178, 0.5000000000000000000 ) ;
#729 = EDGE_LOOP ( 'NONE', ( #5711, #14745, #14272, #12333 ) ) ;
#730 = EDGE_LOOP ( 'NONE', ( #17623, #5630, #1085, #177 ) ) ;
#731 = ORIENTED_EDGE ( 'NONE', *, *, #4525, .F. ) ;
#732 = FACE_OUTER_BOUND ( 'NONE', #9253, .T. ) ;
#733 = CARTESIAN_POINT ( 'NONE',  ( -66.35602477868049220, -15.00000000000001066, -153.7432847437423789 ) ) ;
#734 = CARTESIAN_POINT ( 'NONE',  ( 2.636624412715999011, 2.161493821598055920, -15.91454522070273647 ) ) ;
#735 = CARTESIAN_POINT ( 'NONE',  ( 1.847380140988740260, -11.79969976631074680, 3.949801494731721263 ) ) ;
#736 = CARTESIAN_POINT ( 'NONE',  ( 2.636624412715137922, -14.46769361191291559, 6.973567714907789927 ) ) ;
#737 = CARTESIAN_POINT ( 'NONE',  ( 16.56753206892534891, -0.009389754735541561842, 0.001421777558676752366 ) ) ;
#738 = VECTOR ( 'NONE', #4589, 1000.000000000000227 ) ;
#739 = CARTESIAN_POINT ( 'NONE',  ( 1.918921323896325415, -7.860085869556248994, 9.738309537478970768 ) ) ;
#740 = AXIS2_PLACEMENT_3D ( 'NONE', #14317, #5695, #1124 ) ;
#741 = LINE ( 'NONE', #9527, #14448 ) ;
#742 = CARTESIAN_POINT ( 'NONE',  ( 1.846138399168762101, -12.43476674860266940, 0.4167076046095114505 ) ) ;
#743 = ORIENTED_EDGE ( 'NONE', *, *, #4095, .F. ) ;
#744 = EDGE_CURVE ( 'NONE', #7194, #11848, #2712, .T. ) ;
#745 = EDGE_LOOP ( 'NONE', ( #12051, #16881, #10808, #1545 ) ) ;
#746 = ORIENTED_EDGE ( 'NONE', *, *, #8212, .T. ) ;
#747 = EDGE_CURVE ( 'NONE', #1603, #10624, #8981, .T. ) ;
#748 = VERTEX_POINT ( 'NONE', #3729 ) ;
#749 = DIRECTION ( 'NONE',  ( 0.000000000000000000, 0.000000000000000000, -1.000000000000000000 ) ) ;
#750 = CARTESIAN_POINT ( 'NONE',  ( 1.846138399168762101, 4.238866729160568170, -11.69739621335917690 ) ) ;
#751 = AXIS2_PLACEMENT_3D ( 'NONE', #1811, #13461, #4679 ) ;
#752 = CARTESIAN_POINT ( 'NONE',  ( 0.4862570985993235340, 13.44146924561385958, -3.580942890621532371 ) ) ;
#753 = DIRECTION ( 'NONE',  ( -2.891205793294679312E-16, 1.000000000000000000, -0.000000000000000000 ) ) ;
#754 = DIRECTION ( 'NONE',  ( -1.000000000000000000, -0.000000000000000000, -0.000000000000000000 ) ) ;
#755 = ORIENTED_EDGE ( 'NONE', *, *, #5286, .F. ) ;
#756 = CARTESIAN_POINT ( 'NONE',  ( 1.846524061778021419, 9.853584647934384932, 7.597197846158115553 ) ) ;
#757 = ADVANCED_FACE ( 'NONE', ( #11008 ), #16924, .F. ) ;
#758 = CARTESIAN_POINT ( 'NONE',  ( 2.636624412716913390, 14.14563173255587536, -7.605649742760633991 ) ) ;
#759 = CARTESIAN_POINT ( 'NONE',  ( -5.641944871949442941, 4.153144983957288261, -12.00000000256090260 ) ) ;
#760 = CARTESIAN_POINT ( 'NONE',  ( 0.8740764193769885448, -7.708542792189400750, -12.04241474978016058 ) ) ;
#761 = FACE_OUTER_BOUND ( 'NONE', #16218, .T. ) ;
#762 = CARTESIAN_POINT ( 'NONE',  ( -30.00000000000000355, -12.50000000000000178, 6.500000000000000888 ) ) ;
#763 = LINE ( 'NONE', #18253, #3069 ) ;
#764 =( BOUNDED_SURFACE ( )  B_SPLINE_SURFACE ( 3, 1, ( 
 ( #3424, #12038 ),
 ( #1908, #4772 ),
 ( #378, #16145 ),
 ( #6202, #3224 ) ),
 .UNSPECIFIED., .F., .F., .T. ) 
 B_SPLINE_SURFACE_WITH_KNOTS ( ( 4, 4 ),
 ( 2, 2 ),
 ( 0.000000000000000000, 1.000000000000000000 ),
 ( 0.000000000000000000, 1.000000000000000000 ),
 .UNSPECIFIED. ) 
 GEOMETRIC_REPRESENTATION_ITEM ( )  RATIONAL_B_SPLINE_SURFACE ( (
 ( 1.000000000000000000, 1.000000000000000000),
 ( 0.9933953342250438912, 0.8357391271907739227),
 ( 0.9933953342250438912, 0.8357391271907739227),
 ( 1.000000000000000000, 1.000000000000000000) ) ) 
 REPRESENTATION_ITEM ( '' )  SURFACE ( )  );
#765 = CARTESIAN_POINT ( 'NONE',  ( 2.002547531651519996, 12.17374746633582561, -3.242439124566524278 ) ) ;
#766 = AXIS2_PLACEMENT_3D ( 'NONE', #12959, #3987, #2814 ) ;
#767 = VERTEX_POINT ( 'NONE', #776 ) ;
#768 = VECTOR ( 'NONE', #1333, 1000.000000000000000 ) ;
#770 = ORIENTED_EDGE ( 'NONE', *, *, #1831, .T. ) ;
#769 = CARTESIAN_POINT ( 'NONE',  ( 0.3170788640506441158, 11.20690911610903839, 7.952793437297615675 ) ) ;
#771 = CARTESIAN_POINT ( 'NONE',  ( 2.002547531651519996, -9.778737580845755062, 7.942910686618138705 ) ) ;
#772 = VECTOR ( 'NONE', #8614, 1000.000000000000114 ) ;
#773 = EDGE_CURVE ( 'NONE', #1448, #13827, #16825, .T. ) ;
#774 = B_SPLINE_CURVE_WITH_KNOTS ( 'NONE', 3,
 ( #11173, #9458, #16625, #6498, #10992, #16994 ),
 .UNSPECIFIED., .F., .F.,
 ( 4, 2, 4 ),
 ( 0.000000000000000000, 0.001657017934709842290, 0.003314035869419685448 ),
 .UNSPECIFIED. ) ;
#775 = ORIENTED_EDGE ( 'NONE', *, *, #8349, .F. ) ;
#776 = CARTESIAN_POINT ( 'NONE',  ( 3.950837973638676281, 12.81214529934975310, 6.888253895133341409 ) ) ;
#777 = CARTESIAN_POINT ( 'NONE',  ( -0.7340363079797833645, -6.964562493341727389, -12.00000000352072504 ) ) ;
#778 = ORIENTED_EDGE ( 'NONE', *, *, #1912, .F. ) ;
#779 = CARTESIAN_POINT ( 'NONE',  ( 1.847380140988742925, -7.224522571381399416, 10.13114603776194045 ) ) ;
#780 = CARTESIAN_POINT ( 'NONE',  ( 0.3308579732647023430, -13.25341063505878481, 3.680601586799824076 ) ) ;
#781 = DIRECTION ( 'NONE',  ( 0.000000000000000000, -1.000000000000000000, 0.000000000000000000 ) ) ;
#782 = AXIS2_PLACEMENT_3D ( 'NONE', #11547, #18892, #1309 ) ;
#783 = CARTESIAN_POINT ( 'NONE',  ( -194.9999999999999716, 4.999999999999973355, 6.000000000000000000 ) ) ;
#784 =( NAMED_UNIT ( * ) SI_UNIT ( $, .STERADIAN. ) SOLID_ANGLE_UNIT ( ) );
#785 = CARTESIAN_POINT ( 'NONE',  ( 5.000000000000006217, -30.00000000000000000, 6.000000000000000000 ) ) ;
#786 = CARTESIAN_POINT ( 'NONE',  ( 0.3720661004400040439, 0.7231997263364806638, 13.79610186261030158 ) ) ;
#788 = ORIENTED_EDGE ( 'NONE', *, *, #15085, .T. ) ;
#787 = CARTESIAN_POINT ( 'NONE',  ( 16.56872352241294521, -0.007512283835804365630, 0.007240717549633862542 ) ) ;
#789 = DIRECTION ( 'NONE',  ( 0.000000000000000000, 0.000000000000000000, -1.000000000000000000 ) ) ;
#790 = AXIS2_PLACEMENT_3D ( 'NONE', #1960, #9827, #3474 ) ;
#791 = CARTESIAN_POINT ( 'NONE',  ( 3.950837973638668288, 0.000000000000000000, 0.000000000000000000 ) ) ;
#792 = CARTESIAN_POINT ( 'NONE',  ( 0.3148213771069329203, -10.97836617636219181, -8.260246460850838801 ) ) ;
#793 = CARTESIAN_POINT ( 'NONE',  ( 1.845756295923357104, 11.67600463554279244, -4.296776483139357339 ) ) ;
#794 = PRESENTATION_LAYER_ASSIGNMENT (  '', '', ( #10889 ) ) ;
#795 = EDGE_LOOP ( 'NONE', ( #16035, #279, #1272, #10918 ) ) ;
#796 = VERTEX_POINT ( 'NONE', #15942 ) ;
#797 = CARTESIAN_POINT ( 'NONE',  ( 8.522092701127531811, 2.505958102592620751, 6.489356537178200490 ) ) ;
#798 = CARTESIAN_POINT ( 'NONE',  ( 3.950837973638676281, -6.888253895133199300, -12.81214529934982949 ) ) ;
#799 = VERTEX_POINT ( 'NONE', #10019 ) ;
#800 = FACE_OUTER_BOUND ( 'NONE', #4052, .T. ) ;
#801 = EDGE_CURVE ( 'NONE', #11529, #3711, #15809, .T. ) ;
#802 = CARTESIAN_POINT ( 'NONE',  ( 16.57210152137263393, 0.01402404281923039231, 0.003862718596009517575 ) ) ;
#803 = FACE_OUTER_BOUND ( 'NONE', #16659, .T. ) ;
#804 = CARTESIAN_POINT ( 'NONE',  ( 1.977436885025821267, -1.488549889121935976, 15.33079650480412326 ) ) ;
#805 = LINE ( 'NONE', #12460, #8156 ) ;
#806 = AXIS2_PLACEMENT_3D ( 'NONE', #18244, #754, #1501 ) ;
#807 = LINE ( 'NONE', #18293, #15132 ) ;
#808 = APPLICATION_PROTOCOL_DEFINITION ( 'draft international standard', 'automotive_design', 1998, #5684 ) ;
#809 =( GEOMETRIC_REPRESENTATION_CONTEXT ( 3 ) GLOBAL_UNCERTAINTY_ASSIGNED_CONTEXT ( ( #4439 ) ) GLOBAL_UNIT_ASSIGNED_CONTEXT ( ( #6432, #13867, #784 ) ) REPRESENTATION_CONTEXT ( 'NONE', 'WORKASPACE' ) );
#810 = B_SPLINE_CURVE_WITH_KNOTS ( 'NONE', 3,
 ( #16439, #7455, #17969, #16342, #8967, #13458 ),
 .UNSPECIFIED., .F., .F.,
 ( 4, 2, 4 ),
 ( 2.168404344971008868E-18, 0.001500839035891550922, 0.003001678071783099675 ),
 .UNSPECIFIED. ) ;
#811 = SURFACE_STYLE_USAGE ( .BOTH. , #17931 ) ;
#812 = CARTESIAN_POINT ( 'NONE',  ( 2.002547531651519996, -10.57595306287287329, -6.845637710436306200 ) ) ;
#813 = CARTESIAN_POINT ( 'NONE',  ( 3.512766787570694493, 2.025881399556607843, -14.91422000116826041 ) ) ;
#814 = CARTESIAN_POINT ( 'NONE',  ( 0.3307726912345239634, -12.88561780039862015, 4.812300915532924606 ) ) ;
#815 = DIRECTION ( 'NONE',  ( 0.000000000000000000, 1.000000000000000000, 0.000000000000000000 ) ) ;
#816 = ORIENTED_EDGE ( 'NONE', *, *, #6223, .T. ) ;
#817 = CONICAL_SURFACE ( 'NONE', #14250, 14.54644660717763927, 0.8559913436420816257 ) ;
#818 = ORIENTED_EDGE ( 'NONE', *, *, #17943, .F. ) ;
#819 = VERTEX_POINT ( 'NONE', #14412 ) ;
#820 = ORIENTED_EDGE ( 'NONE', *, *, #18552, .T. ) ;
#821 = CIRCLE ( 'NONE', #5677, 14.54644660717763927 ) ;
#822 = DIRECTION ( 'NONE',  ( -0.4246593920385850485, -0.1376957914266803973, 0.8948208031649685923 ) ) ;
#823 = CARTESIAN_POINT ( 'NONE',  ( 4.195027931520234787, -7.500000000000001776, -16.53644619669688254 ) ) ;
#824 = EDGE_CURVE ( 'NONE', #1293, #8134, #321, .T. ) ;
#825 = CIRCLE ( 'NONE', #211, 5.000000000000004441 ) ;
#826 = APPLICATION_CONTEXT ( 'automotive_design' ) ;
#827 = FACE_OUTER_BOUND ( 'NONE', #6255, .T. ) ;
#828 = DIRECTION ( 'NONE',  ( -1.000000000000000000, 0.000000000000000000, 0.000000000000000000 ) ) ;
#829 = AXIS2_PLACEMENT_3D ( 'NONE', #5389, #17325, #6923 ) ;
#830 = COLOUR_RGB ( '', 0.08235294, 0.09019608, 0.10196078) ;
#831 = DIRECTION ( 'NONE',  ( 1.000000000000000000, 0.000000000000000000, 0.000000000000000000 ) ) ;
#832 = CARTESIAN_POINT ( 'NONE',  ( 0.3058872367615230181, 10.75034008168928068, -8.562166468153600718 ) ) ;
#833 = CARTESIAN_POINT ( 'NONE',  ( 25.00000000000000000, 7.499999999999999112, -16.99999999999999645 ) ) ;
#834 = CLOSED_SHELL ( 'NONE', ( #1353, #12116, #18745, #2158, #7258, #14492, #670, #7285, #7540, #16676, #8621, #13198, #16078, #15978, #14844, #4782, #15344, #6030, #16370, #19, #9913, #896, #16768, #16256, #9026, #12362, #10248, #7370, #18298, #3790, #3520, #8034, #9734, #4930, #9876, #2998, #1892, #1119, #7178, #757, #8644, #16920, #1136, #9988, #15975, #7884, #9819, #14781, #12613, #3497, #3154, #16279, #17386, #4390, #12523, #17725, #13690, #3020, #16226, #6733, #11254, #16175, #6172, #11125, #10141, #8520, #131, #5640, #11541, #12593, #1046, #12070, #11650, #14730, #12238, #7929, #6377, #18616, #49, #16677, #2908, #16030, #11593, #16028, #12458, #14143, #7723, #16173, #15476, #10731, #11016, #15599, #11998, #2570, #2108, #4236, #11894, #11236, #16624, #13067, #10236, #8250, #6292, #12047, #12440, #17515, #10077, #9159, #10235, #15790, #17839, #11761, #1734, #12021, #11256, #2177, #6511, #16100, #1146, #10830, #6605, #5029, #9480, #4853, #17963, #13008, #1691, #8975 ) ) ;
#835 = CARTESIAN_POINT ( 'NONE',  ( 16.56679352167444819, 0.006618561353600086947, 0.006526964904752371663 ) ) ;
#836 = CARTESIAN_POINT ( 'NONE',  ( 15.00000000000000711, -40.00000000000000000, 3.000000000000000000 ) ) ;
#837 = ORIENTED_EDGE ( 'NONE', *, *, #10654, .T. ) ;
#838 = ORIENTED_EDGE ( 'NONE', *, *, #16170, .F. ) ;
#839 = EDGE_LOOP ( 'NONE', ( #9618, #4136, #7135, #7088 ) ) ;
#840 = ORIENTED_EDGE ( 'NONE', *, *, #14124, .T. ) ;
#841 = ORIENTED_EDGE ( 'NONE', *, *, #5974, .T. ) ;
#842 = CARTESIAN_POINT ( 'NONE',  ( 2.636624412717099908, 14.46769361191384817, -6.973567714910368309 ) ) ;
#843 = DIRECTION ( 'NONE',  ( -1.000000000000000000, -0.000000000000000000, -0.000000000000000000 ) ) ;
#844 = PLANE ( 'NONE',  #12960 ) ;
#845 = CARTESIAN_POINT ( 'NONE',  ( 0.3307726912345202441, 13.25328329128666205, 3.680742887039352151 ) ) ;
#846 = VERTEX_POINT ( 'NONE', #13076 ) ;
#847 = EDGE_CURVE ( 'NONE', #1377, #13406, #12495, .T. ) ;
#848 = CARTESIAN_POINT ( 'NONE',  ( 1.847372867223027404, 10.00438561114523850, 7.398914411685026060 ) ) ;
#849 = EDGE_CURVE ( 'NONE', #4916, #18880, #16511, .T. ) ;
#850 = CARTESIAN_POINT ( 'NONE',  ( 0.3137051932979792457, 11.37800749014142276, -7.698472063774345564 ) ) ;
#851 = ADVANCED_FACE ( 'NONE', ( #17477, #10119 ), #8682, .F. ) ;
#852 = CARTESIAN_POINT ( 'NONE',  ( -6.344274892086297690, 2.961199469785570138, -11.99999999981461585 ) ) ;
#853 = CARTESIAN_POINT ( 'NONE',  ( 0.4862570985993235340, -13.89016912371018186, 0.7479633556561964269 ) ) ;
#854 = AXIS2_PLACEMENT_3D ( 'NONE', #15349, #9347, #10785 ) ;
#855 = DIRECTION ( 'NONE',  ( 0.000000000000000000, 0.000000000000000000, 1.000000000000000000 ) ) ;
#856 = DIRECTION ( 'NONE',  ( -0.7561779333270775005, -0.6534392409364822019, 0.03481510524964565034 ) ) ;
#857 = CARTESIAN_POINT ( 'NONE',  ( 1.254255976357841584, 1.011593778944668731, -14.64488542023482331 ) ) ;
#858 = DIRECTION ( 'NONE',  ( -1.000000000000000000, -0.000000000000000000, -0.000000000000000000 ) ) ;
#859 = VERTEX_POINT ( 'NONE', #1324 ) ;
#861 = ORIENTED_EDGE ( 'NONE', *, *, #15792, .T. ) ;
#860 = DIRECTION ( 'NONE',  ( 1.000000000000000000, 0.000000000000000000, -0.000000000000000000 ) ) ;
#862 = LINE ( 'NONE', #2380, #530 ) ;
#863 = PLANE ( 'NONE',  #7082 ) ;
#864 = VECTOR ( 'NONE', #14123, 1000.000000000000000 ) ;
#865 = ORIENTED_EDGE ( 'NONE', *, *, #8599, .F. ) ;
#866 = CARTESIAN_POINT ( 'NONE',  ( 3.950837973638677170, 6.316429227969654114, -13.10350451991833687 ) ) ;
#867 = CARTESIAN_POINT ( 'NONE',  ( -6.108979705494616219, -3.422227477007855789, -11.99999999936559902 ) ) ;
#868 = ORIENTED_EDGE ( 'NONE', *, *, #18008, .F. ) ;
#869 = CARTESIAN_POINT ( 'NONE',  ( -31.48433267924924550, 17.77350098112614418, 3.000000000000000000 ) ) ;
#870 = CARTESIAN_POINT ( 'NONE',  ( 0.3939875929385635023, 13.80036004410494499, -0.7003304234513649806 ) ) ;
#871 = CARTESIAN_POINT ( 'NONE',  ( 8.438534575730034959, -6.862570336891073985, -0.2320579683290849293 ) ) ;
#872 = CARTESIAN_POINT ( 'NONE',  ( 3.512766787570764215, -6.535475144497081779, 13.55823433651946175 ) ) ;
#873 =( BOUNDED_SURFACE ( )  B_SPLINE_SURFACE ( 3, 1, ( 
 ( #8225, #3999 ),
 ( #4452, #18426 ),
 ( #6786, #11366 ),
 ( #2648, #1494 ) ),
 .UNSPECIFIED., .F., .F., .T. ) 
 B_SPLINE_SURFACE_WITH_KNOTS ( ( 4, 4 ),
 ( 2, 2 ),
 ( 0.000000000000000000, 1.000000000000000000 ),
 ( 0.000000000000000000, 1.000000000000000000 ),
 .UNSPECIFIED. ) 
 GEOMETRIC_REPRESENTATION_ITEM ( )  RATIONAL_B_SPLINE_SURFACE ( (
 ( 1.000000000000000000, 1.000000000000000000),
 ( 0.7792777138730158093, 0.9689936506012928330),
 ( 0.7792777138730158093, 0.9689936506012928330),
 ( 1.000000000000000000, 1.000000000000000000) ) ) 
 REPRESENTATION_ITEM ( '' )  SURFACE ( )  );
#874 = CARTESIAN_POINT ( 'NONE',  ( 0.000000000000000000, 0.000000000000000000, 11.00000000000000000 ) ) ;
#875 = EDGE_CURVE ( 'NONE', #12927, #9066, #3498, .T. ) ;
#876 = CARTESIAN_POINT ( 'NONE',  ( 20.00000000000000000, 2.499999999999998668, -17.00000000000000000 ) ) ;
#877 = CARTESIAN_POINT ( 'NONE',  ( 16.56753206892534891, 0.009389754735541551434, -0.001421777558676823056 ) ) ;
#879 = VERTEX_POINT ( 'NONE', #5706 ) ;
#878 = CARTESIAN_POINT ( 'NONE',  ( 16.56822296793089322, -0.006547366384935564970, 0.007741272030791060237 ) ) ;
#880 = DIRECTION ( 'NONE',  ( 1.000000000000000000, 1.298018465182616140E-16, 0.000000000000000000 ) ) ;
#881 = FACE_OUTER_BOUND ( 'NONE', #10478, .T. ) ;
#882 = CARTESIAN_POINT ( 'NONE',  ( 0.3132635586635975078, 8.495712071659401232, 10.79541209008106861 ) ) ;
#883 = CARTESIAN_POINT ( 'NONE',  ( 0.3142011359265305392, -4.608101617236689762, -12.94258167753017297 ) ) ;
#884 = EDGE_LOOP ( 'NONE', ( #132, #11644, #15801, #8362 ) ) ;
#885 = VERTEX_POINT ( 'NONE', #18534 ) ;
#886 = CARTESIAN_POINT ( 'NONE',  ( 1.918918678667045130, -9.738328798462433156, 7.860057224348805605 ) ) ;
#887 = ORIENTED_EDGE ( 'NONE', *, *, #17637, .T. ) ;
#888 = CARTESIAN_POINT ( 'NONE',  ( 2.002547531651519996, -0.6781519942170860515, -12.57989064830760206 ) ) ;
#889 = CARTESIAN_POINT ( 'NONE',  ( 1.918918678667045130, 6.832809802519163256, -10.48466773720554279 ) ) ;
#890 = PRODUCT_RELATED_PRODUCT_CATEGORY ( 'part', '', ( #3248 ) ) ;
#891 = CARTESIAN_POINT ( 'NONE',  ( 1.847380140988742703, -10.13114603776191380, -7.224522571381438496 ) ) ;
#892 =( GEOMETRIC_REPRESENTATION_CONTEXT ( 3 ) GLOBAL_UNCERTAINTY_ASSIGNED_CONTEXT ( ( #13048 ) ) GLOBAL_UNIT_ASSIGNED_CONTEXT ( ( #18467, #18375, #3851 ) ) REPRESENTATION_CONTEXT ( 'NONE', 'WORKASPACE' ) );
#893 = EDGE_CURVE ( 'NONE', #11930, #15939, #2932, .T. ) ;
#894 = CARTESIAN_POINT ( 'NONE',  ( 1.959212340397961327, 12.53706137681889743, 0.6675998551412224424 ) ) ;
#895 = DIRECTION ( 'NONE',  ( -1.000000000000000000, -0.000000000000000000, -0.000000000000000000 ) ) ;
#896 = ADVANCED_FACE ( 'NONE', ( #11558 ), #16489, .T. ) ;
#897 = CARTESIAN_POINT ( 'NONE',  ( 1.977228804422058728, -14.12033626431055211, 6.152949558601312319 ) ) ;
#898 = APPLICATION_PROTOCOL_DEFINITION ( 'draft international standard', 'automotive_design', 1998, #14485 ) ;
#899 = AXIS2_PLACEMENT_3D ( 'NONE', #17631, #10363, #9124 ) ;
#900 = SURFACE_STYLE_USAGE ( .BOTH. , #17132 ) ;
#901 = CARTESIAN_POINT ( 'NONE',  ( 16.56872352241294521, 0.007512283835805451566, 0.007240717549634016065 ) ) ;
#902 = DIRECTION ( 'NONE',  ( 0.000000000000000000, 0.000000000000000000, -1.000000000000000000 ) ) ;
#903 = DIRECTION ( 'NONE',  ( 0.000000000000000000, 0.000000000000000000, 1.000000000000000000 ) ) ;
#904 = CARTESIAN_POINT ( 'NONE',  ( 15.00000000000000711, -24.99999999999999645, 6.000000000000000000 ) ) ;
#905 = VECTOR ( 'NONE', #16915, 1000.000000000000114 ) ;
#906 = CARTESIAN_POINT ( 'NONE',  ( 1.254009781011930613, -12.44229282923100932, -7.789615163754561422 ) ) ;
#907 = CARTESIAN_POINT ( 'NONE',  ( 0.3095370825347224519, -4.681152801286251552, 12.91933430393606486 ) ) ;
#908 = ORIENTED_EDGE ( 'NONE', *, *, #17596, .T. ) ;
#909 = EDGE_CURVE ( 'NONE', #12106, #1319, #1522, .T. ) ;
#910 = ORIENTED_EDGE ( 'NONE', *, *, #9287, .F. ) ;
#911 = VERTEX_POINT ( 'NONE', #7070 ) ;
#912 = ORIENTED_EDGE ( 'NONE', *, *, #7530, .F. ) ;
#913 = VERTEX_POINT ( 'NONE', #1138 ) ;
#914 = CARTESIAN_POINT ( 'NONE',  ( 2.636624412716045196, 11.10302021257998994, -11.60464335004042447 ) ) ;
#915 = CARTESIAN_POINT ( 'NONE',  ( -4.160991745704744282, -7.500000000000002665, -16.52287405655582475 ) ) ;
#916 = DIRECTION ( 'NONE',  ( 0.7635533937278214944, -0.5095610256143857653, -0.3966532189476615899 ) ) ;
#917 = CARTESIAN_POINT ( 'NONE',  ( 1.254009781011619307, -7.789615163754444183, 12.44229282923071445 ) ) ;
#918 = CARTESIAN_POINT ( 'NONE',  ( 16.57778382496167424, -0.007244066302946679421, -0.01306626476309297180 ) ) ;
#919 = CARTESIAN_POINT ( 'NONE',  ( 16.56753206892534891, -0.008432171035096412345, -0.004368917149004214288 ) ) ;
#920 = CARTESIAN_POINT ( 'NONE',  ( 16.56872352241294521, -0.004907101719995745834, -0.009207754980064182873 ) ) ;
#921 = LINE ( 'NONE', #8015, #14130 ) ;
#922 = EDGE_CURVE ( 'NONE', #2319, #4709, #14420, .T. ) ;
#923 = CARTESIAN_POINT ( 'NONE',  ( 1.342453679581834924, -14.34050741580209198, 3.649820028552675844 ) ) ;
#924 = ORIENTED_EDGE ( 'NONE', *, *, #7440, .T. ) ;
#925 = ORIENTED_EDGE ( 'NONE', *, *, #8906, .T. ) ;
#926 = EDGE_CURVE ( 'NONE', #14041, #17093, #6983, .T. ) ;
#927 = ORIENTED_EDGE ( 'NONE', *, *, #160, .T. ) ;
#928 = ORIENTED_EDGE ( 'NONE', *, *, #4691, .F. ) ;
#929 = CIRCLE ( 'NONE', #5160, 16.06066017081991149 ) ;
#930 = CARTESIAN_POINT ( 'NONE',  ( 1.342453679581834924, 12.51077660954466353, 7.902645620902494450 ) ) ;
#931 = DIRECTION ( 'NONE',  ( -0.000000000000000000, -0.000000000000000000, 1.000000000000000000 ) ) ;
#932 = DIRECTION ( 'NONE',  ( -1.000000000000000000, 0.000000000000000000, 0.000000000000000000 ) ) ;
#933 = CARTESIAN_POINT ( 'NONE',  ( 0.3095370825347234511, -8.444334731364085300, 10.84046130709055333 ) ) ;
#934 = CARTESIAN_POINT ( 'NONE',  ( 1.846138399168762101, -6.971848976711082280, 10.30487220521567693 ) ) ;
#935 = ORIENTED_EDGE ( 'NONE', *, *, #13033, .T. ) ;
#936 = CARTESIAN_POINT ( 'NONE',  ( 0.4862570985993235340, -7.559321496869506163, 11.67702470553362559 ) ) ;
#937 = CARTESIAN_POINT ( 'NONE',  ( 8.522092701127531811, -6.946128462138593029, -0.3779863304871954321 ) ) ;
#938 = CARTESIAN_POINT ( 'NONE',  ( 6.453131650770538741, 2.715944631655133001, -12.00000000019078428 ) ) ;
#939 = CARTESIAN_POINT ( 'NONE',  ( 1.846138399168762101, -11.95493567637848109, -3.446241763653124401 ) ) ;
#940 = FACE_OUTER_BOUND ( 'NONE', #15985, .T. ) ;
#941 = CARTESIAN_POINT ( 'NONE',  ( 1.847380140988742925, 3.949801494731767892, 11.79969976631073081 ) ) ;
#942 = DIRECTION ( 'NONE',  ( -0.000000000000000000, -0.000000000000000000, -1.000000000000000000 ) ) ;
#943 = B_SPLINE_CURVE_WITH_KNOTS ( 'NONE', 3,
 ( #16001, #4262, #13232, #5970, #8747, #11615 ),
 .UNSPECIFIED., .F., .F.,
 ( 4, 2, 4 ),
 ( 4.027530160694267299E-17, 0.0002014099069817290827, 0.0004028198139634178872 ),
 .UNSPECIFIED. ) ;
#944 = CARTESIAN_POINT ( 'NONE',  ( 2.320520222539219635, -3.126729907238178896, -15.43440824796753930 ) ) ;
#945 = ORIENTED_EDGE ( 'NONE', *, *, #13952, .T. ) ;
#947 = ORIENTED_EDGE ( 'NONE', *, *, #11281, .T. ) ;
#946 = FACE_OUTER_BOUND ( 'NONE', #11798, .T. ) ;
#948 = CARTESIAN_POINT ( 'NONE',  ( 16.56872352241294521, 0.009207754980064196751, -0.004907101719995712874 ) ) ;
#949 = EDGE_CURVE ( 'NONE', #14986, #8583, #5172, .T. ) ;
#950 = EDGE_CURVE ( 'NONE', #9697, #3395, #3249, .T. ) ;
#951 = EDGE_CURVE ( 'NONE', #11815, #17865, #15847, .T. ) ;
#952 = AXIS2_PLACEMENT_3D ( 'NONE', #17004, #15642, #4089 ) ;
#953 = DIRECTION ( 'NONE',  ( 0.000000000000000000, -1.000000000000000000, 0.000000000000000000 ) ) ;
#954 = ORIENTED_EDGE ( 'NONE', *, *, #11160, .F. ) ;
#955 = CARTESIAN_POINT ( 'NONE',  ( 0.3058872367615230181, 11.46514199369357989, 7.578326039752647958 ) ) ;
#956 = B_SPLINE_CURVE_WITH_KNOTS ( 'NONE', 3,
 ( #2833, #10120, #14163, #5806, #11653, #17478 ),
 .UNSPECIFIED., .F., .F.,
 ( 4, 2, 4 ),
 ( 8.673617379884035472E-19, 0.001500839035891551789, 0.003001678071783102711 ),
 .UNSPECIFIED. ) ;
#957 = LINE ( 'NONE', #18435, #5032 ) ;
#958 = ORIENTED_EDGE ( 'NONE', *, *, #8263, .F. ) ;
#959 = CARTESIAN_POINT ( 'NONE',  ( 2.636624412715138366, -11.10302021257964888, 11.60464335004044223 ) ) ;
#960 = CARTESIAN_POINT ( 'NONE',  ( 4.755015822784811164, -4.336808689942017736E-16, 0.000000000000000000 ) ) ;
#961 = CARTESIAN_POINT ( 'NONE',  ( 0.3307726912345201886, -8.558645027434195640, -10.76786801061216714 ) ) ;
#962 = EDGE_CURVE ( 'NONE', #767, #9990, #14479, .T. ) ;
#963 = LINE ( 'NONE', #3481, #18162 ) ;
#964 = VECTOR ( 'NONE', #10328, 1000.000000000000000 ) ;
#965 = PRESENTATION_STYLE_ASSIGNMENT (( #14060 ) ) ;
#966 = CARTESIAN_POINT ( 'NONE',  ( 2.123976203522053741, -14.31368049382974483, 6.261444813538503240 ) ) ;
#967 = CARTESIAN_POINT ( 'NONE',  ( 0.3058872367615230181, -10.75034008168922206, 8.562166468153680654 ) ) ;
#969 = EDGE_LOOP ( 'NONE', ( #5849, #9714, #10891, #1040, #8292, #7403 ) ) ;
#968 = DIRECTION ( 'NONE',  ( 1.000000000000000000, 0.000000000000000000, 0.000000000000000000 ) ) ;
#970 = CARTESIAN_POINT ( 'NONE',  ( 16.56679352167444819, 0.008311568981097982450, 0.004162264567718830001 ) ) ;
#971 = ORIENTED_EDGE ( 'NONE', *, *, #14652, .T. ) ;
#972 = DIRECTION ( 'NONE',  ( -1.000000000000000000, -0.000000000000000000, -0.000000000000000000 ) ) ;
#973 = FACE_OUTER_BOUND ( 'NONE', #8848, .T. ) ;
#974 = ORIENTED_EDGE ( 'NONE', *, *, #1070, .T. ) ;
#975 = DIRECTION ( 'NONE',  ( 0.7561779333270775005, 0.4122479608995740508, -0.5081796452863232005 ) ) ;
#976 = ADVANCED_FACE ( 'NONE', ( #6303 ), #14988, .F. ) ;
#977 = CARTESIAN_POINT ( 'NONE',  ( 0.3145734862173240054, 0.3064017202077272128, -13.73540602248380971 ) ) ;
#978 = VERTEX_POINT ( 'NONE', #4488 ) ;
#979 = LINE ( 'NONE', #3397, #6527 ) ;
#980 = CARTESIAN_POINT ( 'NONE',  ( 16.57210152137263393, -0.005118120558001483002, 0.01361613799508852585 ) ) ;
#981 = AXIS2_PLACEMENT_3D ( 'NONE', #15850, #2740, #2928 ) ;
#982 = DIRECTION ( 'NONE',  ( -0.7561779333270775005, 0.5491072561318340872, 0.3559159372837335522 ) ) ;
#983 = CARTESIAN_POINT ( 'NONE',  ( -4.999999999999995559, -30.00000000000000000, 26.00000000000000000 ) ) ;
#984 = EDGE_CURVE ( 'NONE', #4000, #3723, #9255, .T. ) ;
#985 = SHAPE_DEFINITION_REPRESENTATION ( #14856, #9604 ) ;
#986 = APPLICATION_PROTOCOL_DEFINITION ( 'draft international standard', 'automotive_design', 1998, #2754 ) ;
#987 = CARTESIAN_POINT ( 'NONE',  ( 0.3095370825347233956, 7.700448427572036181, -11.38092634279620263 ) ) ;
#988 = DIRECTION ( 'NONE',  ( 1.000000000000000000, 0.000000000000000000, -0.000000000000000000 ) ) ;
#989 = B_SPLINE_CURVE_WITH_KNOTS ( 'NONE', 3,
 ( #17211, #10142, #15779, #11770, #8804, #17501, #5542, #15966, #2579, #2957, #11393, #8425, #12910 ),
 .UNSPECIFIED., .F., .F.,
 ( 4, 3, 3, 3, 4 ),
 ( 4.670885906470169154E-18, 0.0002299780670421063087, 0.0004599561239687901203, 0.0006896788984287873046, 0.0009194956271626388705 ),
 .UNSPECIFIED. ) ;
#990 = CARTESIAN_POINT ( 'NONE',  ( 1.846822687350019310, -3.566003975885607691, -11.92063725419902731 ) ) ;
#991 = CARTESIAN_POINT ( 'NONE',  ( 16.56872352241294521, -0.004564908236400289435, -0.009382111268606239951 ) ) ;
#992 =( LENGTH_UNIT ( ) NAMED_UNIT ( * ) SI_UNIT ( .MILLI., .METRE. ) );
#993 = B_SPLINE_CURVE_WITH_KNOTS ( 'NONE', 3,
 ( #12995, #11576, #11764, #5628, #7376, #11481, #18728, #17394, #13186, #1623, #14813, #17592, #1725 ),
 .UNSPECIFIED., .F., .F.,
 ( 4, 3, 3, 3, 4 ),
 ( 0.000000000000000000, 0.0002299804304191490972, 0.0004599608082120256055, 0.0006467586077648033180, 0.0008336169836825999165 ),
 .UNSPECIFIED. ) ;
#994 = ORIENTED_EDGE ( 'NONE', *, *, #17881, .T. ) ;
#995 = ORIENTED_EDGE ( 'NONE', *, *, #893, .T. ) ;
#996 = VERTEX_POINT ( 'NONE', #10503 ) ;
#997 = ORIENTED_EDGE ( 'NONE', *, *, #13718, .T. ) ;
#998 = VERTEX_POINT ( 'NONE', #13172 ) ;
#999 = AXIS2_PLACEMENT_3D ( 'NONE', #650, #13915, #13738 ) ;
#1000 = CARTESIAN_POINT ( 'NONE',  ( 1.847340342630335641, -0.1245571717074845930, -12.44248139376885831 ) ) ;
#1001 = EDGE_CURVE ( 'NONE', #1902, #7915, #810, .T. ) ;
#1002 = CARTESIAN_POINT ( 'NONE',  ( 0.3142011359265314829, 12.94258167753018895, -4.608101617236642689 ) ) ;
#1003 = CARTESIAN_POINT ( 'NONE',  ( 2.697797270744668019, 7.053988368581864066, 11.26906156738829168 ) ) ;
#1004 = EDGE_CURVE ( 'NONE', #2340, #1302, #7798, .T. ) ;
#1005 = CARTESIAN_POINT ( 'NONE',  ( 0.3095370825347234511, -10.84046130709052314, -8.444334731364126156 ) ) ;
#1006 = CARTESIAN_POINT ( 'NONE',  ( 0.3151928479966097374, 0.000000000000000000, -13.73922861026898623 ) ) ;
#1007 = CARTESIAN_POINT ( 'NONE',  ( 0.4754618798421167414, 0.7484603771386338922, -13.89949764182681768 ) ) ;
#1008 = CARTESIAN_POINT ( 'NONE',  ( 16.57210152137263393, 0.01214401161737518019, -0.008007331252332923130 ) ) ;
#1009 = AXIS2_PLACEMENT_3D ( 'NONE', #5627, #10227, #11663 ) ;
#1010 = ORIENTED_EDGE ( 'NONE', *, *, #143, .T. ) ;
#1011 = ORIENTED_EDGE ( 'NONE', *, *, #18077, .T. ) ;
#1012 = VERTEX_POINT ( 'NONE', #12034 ) ;
#1013 = EDGE_LOOP ( 'NONE', ( #6633, #16356, #12119, #12291 ) ) ;
#1014 = CARTESIAN_POINT ( 'NONE',  ( 1.847412631396506022, 3.886120457021560171, -11.82061107079959861 ) ) ;
#1015 = DIRECTION ( 'NONE',  ( 0.000000000000000000, 0.000000000000000000, 1.000000000000000000 ) ) ;
#1016 = CARTESIAN_POINT ( 'NONE',  ( 1.959283090834842200, -11.71721539537258394, 4.509128209890929107 ) ) ;
#1017 = CARTESIAN_POINT ( 'NONE',  ( -194.9999999999999716, 4.999999999999973355, 11.00000000000000000 ) ) ;
#1018 = CARTESIAN_POINT ( 'NONE',  ( 1.342453679581834924, -3.649820028552632767, -14.34050741580210619 ) ) ;
#1019 = ORIENTED_EDGE ( 'NONE', *, *, #3155, .F. ) ;
#1020 = EDGE_CURVE ( 'NONE', #2439, #16598, #1609, .T. ) ;
#1021 = CARTESIAN_POINT ( 'NONE',  ( 1.846955891736118849, -11.91257079808165820, -3.593597880662470878 ) ) ;
#1022 = VECTOR ( 'NONE', #16046, 1000.000000000000114 ) ;
#1023 = LINE ( 'NONE', #11358, #11282 ) ;
#1024 = CARTESIAN_POINT ( 'NONE',  ( 1.845755665166724624, -7.694641135842892332, 9.776700214453605042 ) ) ;
#1025 = CARTESIAN_POINT ( 'NONE',  ( 1.845755665166725068, 11.97169564665396280, -3.386720041070604204 ) ) ;
#1026 = ADVANCED_FACE ( 'NONE', ( #14896 ), #12138, .T. ) ;
#1027 = DIRECTION ( 'NONE',  ( -1.000000000000000000, 0.000000000000000000, 0.000000000000000000 ) ) ;
#1028 = CARTESIAN_POINT ( 'NONE',  ( 16.56872352241294521, 0.01033355228142401709, -0.001442253899401843694 ) ) ;
#1029 = CARTESIAN_POINT ( 'NONE',  ( 1.846524061778020531, -4.180439405448407975, 11.71897913237548039 ) ) ;
#1030 = ORIENTED_EDGE ( 'NONE', *, *, #3955, .F. ) ;
#1032 = ORIENTED_EDGE ( 'NONE', *, *, #11354, .T. ) ;
#1031 = FACE_OUTER_BOUND ( 'NONE', #18121, .T. ) ;
#1033 = CARTESIAN_POINT ( 'NONE',  ( 16.57778382496167424, 0.002851818597093999999, -0.01466529584256785410 ) ) ;
#1034 = CIRCLE ( 'NONE', #6558, 5.000000000000000888 ) ;
#1035 = CYLINDRICAL_SURFACE ( 'NONE', #4951, 5.000000000000000000 ) ;
#1036 = VERTEX_POINT ( 'NONE', #9164 ) ;
#1037 = CARTESIAN_POINT ( 'NONE',  ( 2.002547531651519996, 12.57989064830759496, -0.6781519942172177240 ) ) ;
#1038 = CARTESIAN_POINT ( 'NONE',  ( -6.538348415310826667, -7.500000000000000888, -17.00000000000000000 ) ) ;
#1039 = LINE ( 'NONE', #4919, #11473 ) ;
#1040 = ORIENTED_EDGE ( 'NONE', *, *, #8176, .F. ) ;
#1041 = CARTESIAN_POINT ( 'NONE',  ( 1.977436885026095270, -10.21547824869579202, 11.52792723756318694 ) ) ;
#1042 = DIRECTION ( 'NONE',  ( -1.000000000000000000, -0.000000000000000000, -0.000000000000000000 ) ) ;
#1043 = CARTESIAN_POINT ( 'NONE',  ( 2.749999999999997335, 0.000000000000000000, 7.000000000000000000 ) ) ;
#1044 = CARTESIAN_POINT ( 'NONE',  ( 3.950837973638668288, 0.000000000000000000, 0.000000000000000000 ) ) ;
#1045 = AXIS2_PLACEMENT_3D ( 'NONE', #18602, #5505, #11353 ) ;
#1046 = ADVANCED_FACE ( 'NONE', ( #3123 ), #9224, .F. ) ;
#1047 = CARTESIAN_POINT ( 'NONE',  ( 3.512766787570752669, -14.91422000116822311, 2.025881399556336060 ) ) ;
#1048 = EDGE_CURVE ( 'NONE', #8831, #8605, #1481, .T. ) ;
#1049 = AXIS2_PLACEMENT_3D ( 'NONE', #1810, #12037, #17872 ) ;
#1050 = FILL_AREA_STYLE ('',( #5450 ) ) ;
#1051 = DIRECTION ( 'NONE',  ( -0.7635533937278214944, -0.1790966170213966202, 0.6204116510013472086 ) ) ;
#1052 = B_SPLINE_CURVE_WITH_KNOTS ( 'NONE', 3,
 ( #4893, #6326, #3442, #7765, #17986, #9278 ),
 .UNSPECIFIED., .F., .F.,
 ( 4, 2, 4 ),
 ( 3.903127820947815962E-18, 0.0002017457492448081235, 0.0004034914984896123438 ),
 .UNSPECIFIED. ) ;
#1053 = CARTESIAN_POINT ( 'NONE',  ( -194.9999999999999716, -15.00000000000003020, -153.7432847437423789 ) ) ;
#1055 = ORIENTED_EDGE ( 'NONE', *, *, #4349, .F. ) ;
#1054 = DIRECTION ( 'NONE',  ( -1.000000000000000000, 0.000000000000000000, 0.000000000000000000 ) ) ;
#1056 = DIRECTION ( 'NONE',  ( 0.000000000000000000, 0.000000000000000000, -1.000000000000000000 ) ) ;
#1057 = CARTESIAN_POINT ( 'NONE',  ( 0.3151930723728408879, -13.04315954105012310, -4.318364831037728280 ) ) ;
#1058 = CARTESIAN_POINT ( 'NONE',  ( 0.3151928476913619104, -4.245853234426296474, -13.06671852871093265 ) ) ;
#1059 = ORIENTED_EDGE ( 'NONE', *, *, #6680, .F. ) ;
#1060 = DIRECTION ( 'NONE',  ( -0.7561779333270775005, 0.2350349629540185170, 0.6106991889125065187 ) ) ;
#1061 = CARTESIAN_POINT ( 'NONE',  ( 3.512766787570756222, -14.81029789862160762, 2.682019731918325878 ) ) ;
#1062 = VECTOR ( 'NONE', #916, 1000.000000000000227 ) ;
#1063 = ORIENTED_EDGE ( 'NONE', *, *, #56, .F. ) ;
#1064 = CARTESIAN_POINT ( 'NONE',  ( 3.512766787570762439, -10.40533104696141997, 10.87507422923886224 ) ) ;
#1065 = CIRCLE ( 'NONE', #13280, 7.000000000000000000 ) ;
#1066 =( NAMED_UNIT ( * ) SI_UNIT ( $, .STERADIAN. ) SOLID_ANGLE_UNIT ( ) );
#1067 = CARTESIAN_POINT ( 'NONE',  ( 8.438534575730034959, -2.341351102130323714, 6.454982381540280478 ) ) ;
#1068 = CARTESIAN_POINT ( 'NONE',  ( 1.846138399168762101, 7.646096044340033870, -9.815003036200328879 ) ) ;
#1069 = CARTESIAN_POINT ( 'NONE',  ( 3.950837973638675393, -10.51028938476224894, 10.05648675950122595 ) ) ;
#1070 = EDGE_CURVE ( 'NONE', #17590, #5950, #14707, .T. ) ;
#1071 = EDGE_CURVE ( 'NONE', #8960, #9141, #6112, .T. ) ;
#1072 = VERTEX_POINT ( 'NONE', #12228 ) ;
#1073 = EDGE_CURVE ( 'NONE', #15587, #15699, #16006, .T. ) ;
#1074 = SHAPE_DEFINITION_REPRESENTATION ( #9384, #14244 ) ;
#1075 = CARTESIAN_POINT ( 'NONE',  ( 0.3307726912345229087, -13.25328329128663007, -3.680742887039447631 ) ) ;
#1076 = CARTESIAN_POINT ( 'NONE',  ( 2.002547531651519996, -3.242439124566566910, -12.17374746633581495 ) ) ;
#1077 = CIRCLE ( 'NONE', #5966, 7.000000000000000000 ) ;
#1078 = CARTESIAN_POINT ( 'NONE',  ( 1.847461586945734480, -3.877048136045296634, -11.82388984758122596 ) ) ;
#1079 = CARTESIAN_POINT ( 'NONE',  ( 1.846955891736119293, 4.094751675596701723, 11.74973605926565767 ) ) ;
#1080 = CARTESIAN_POINT ( 'NONE',  ( 2.750000000000000000, 0.000000000000000000, 10.00000000000000000 ) ) ;
#1081 = ORIENTED_EDGE ( 'NONE', *, *, #10539, .F. ) ;
#1082 = LINE ( 'NONE', #2506, #14552 ) ;
#1083 = CARTESIAN_POINT ( 'NONE',  ( 1.861706995891668326, -7.751853334747247359, -9.751699138048525839 ) ) ;
#1084 = ORIENTED_EDGE ( 'NONE', *, *, #2353, .T. ) ;
#1085 = ORIENTED_EDGE ( 'NONE', *, *, #8263, .T. ) ;
#1086 = ORIENTED_EDGE ( 'NONE', *, *, #10179, .T. ) ;
#1087 = VERTEX_POINT ( 'NONE', #8024 ) ;
#1088 = AXIS2_PLACEMENT_3D ( 'NONE', #17339, #4255, #4345 ) ;
#1089 =( GEOMETRIC_REPRESENTATION_CONTEXT ( 3 ) GLOBAL_UNCERTAINTY_ASSIGNED_CONTEXT ( ( #4604 ) ) GLOBAL_UNIT_ASSIGNED_CONTEXT ( ( #12759, #3971, #14471 ) ) REPRESENTATION_CONTEXT ( 'NONE', 'WORKASPACE' ) );
#1090 = CARTESIAN_POINT ( 'NONE',  ( 0.3307726912345202441, 13.25328329128666205, 3.680742887039352151 ) ) ;
#1091 = FACE_OUTER_BOUND ( 'NONE', #11796, .T. ) ;
#1092 = VECTOR ( 'NONE', #2228, 1000.000000000000114 ) ;
#1093 = FACE_OUTER_BOUND ( 'NONE', #18260, .T. ) ;
#1094 = CARTESIAN_POINT ( 'NONE',  ( 2.747332970342022840, 7.555624153089646633, 14.49942876448594831 ) ) ;
#1095 = CARTESIAN_POINT ( 'NONE',  ( 2.636624412715362631, -15.80357026013197519, 2.862162146984090327 ) ) ;
#1096 = DIRECTION ( 'NONE',  ( 0.000000000000000000, 0.000000000000000000, -1.000000000000000000 ) ) ;
#1097 = CARTESIAN_POINT ( 'NONE',  ( 16.58200780006414732, -0.007066318000004643239, -0.008650561019685603162 ) ) ;
#1098 = EDGE_CURVE ( 'NONE', #18405, #4361, #3805, .T. ) ;
#1099 = CARTESIAN_POINT ( 'NONE',  ( 0.3145734862173208413, -13.15783074029281963, 3.953068532979947314 ) ) ;
#1100 = CARTESIAN_POINT ( 'NONE',  ( 2.002547531651519996, -12.57989064830760206, 0.6781519942171299054 ) ) ;
#1101 = ORIENTED_EDGE ( 'NONE', *, *, #3756, .F. ) ;
#1102 =( GEOMETRIC_REPRESENTATION_CONTEXT ( 3 ) GLOBAL_UNCERTAINTY_ASSIGNED_CONTEXT ( ( #11702 ) ) GLOBAL_UNIT_ASSIGNED_CONTEXT ( ( #6049, #7298, #13114 ) ) REPRESENTATION_CONTEXT ( 'NONE', 'WORKASPACE' ) );
#1103 = VERTEX_POINT ( 'NONE', #750 ) ;
#1104 = ORIENTED_EDGE ( 'NONE', *, *, #11705, .T. ) ;
#1105 = EDGE_LOOP ( 'NONE', ( #13101, #4621, #16613, #14738 ) ) ;
#1106 = DIRECTION ( 'NONE',  ( -0.000000000000000000, 1.000000000000000000, 0.000000000000000000 ) ) ;
#1107 = B_SPLINE_CURVE_WITH_KNOTS ( 'NONE', 3,
 ( #17995, #872, #508, #12167 ),
 .UNSPECIFIED., .F., .F.,
 ( 4, 4 ),
 ( 0.000000000000000000, 0.002004993803842710330 ),
 .UNSPECIFIED. ) ;
#1108 = ADVANCED_FACE ( 'NONE', ( #11167 ), #6399, .F. ) ;
#1109 = CARTESIAN_POINT ( 'NONE',  ( 2.353870697619111496, 12.53036919722789477, -3.268530966681500782 ) ) ;
#1110 = CARTESIAN_POINT ( 'NONE',  ( 1.846822687350017311, 10.23524390843949483, -7.075150813727003829 ) ) ;
#1111 = LINE ( 'NONE', #8383, #16047 ) ;
#1112 = ORIENTED_EDGE ( 'NONE', *, *, #15678, .T. ) ;
#1113 = CARTESIAN_POINT ( 'NONE',  ( 0.3720661004400037664, 8.694226082900744501, -10.73619472937692620 ) ) ;
#1114 = AXIS2_PLACEMENT_3D ( 'NONE', #3088, #8932, #9328 ) ;
#1115 = CARTESIAN_POINT ( 'NONE',  ( 2.002547531651519996, -12.17374746633580784, 3.242439124566603326 ) ) ;
#1116 = CARTESIAN_POINT ( 'NONE',  ( 5.926008024970927934, 7.499999999999999112, -16.97528233579637558 ) ) ;
#1117 = LINE ( 'NONE', #7347, #12489 ) ;
#1118 = MECHANICAL_DESIGN_GEOMETRIC_PRESENTATION_REPRESENTATION (  '', ( #6327 ), #6934 ) ;
#1119 = ADVANCED_FACE ( 'NONE', ( #3523 ), #7277, .F. ) ;
#1120 = EDGE_CURVE ( 'NONE', #13188, #8612, #18448, .T. ) ;
#1121 = AXIS2_PLACEMENT_3D ( 'NONE', #8036, #5424, #9728 ) ;
#1122 = CARTESIAN_POINT ( 'NONE',  ( 2.636624412714237309, 15.80357026013209953, 2.862162146984226663 ) ) ;
#1123 = AXIS2_PLACEMENT_3D ( 'NONE', #6884, #14137, #3641 ) ;
#1124 = DIRECTION ( 'NONE',  ( 0.000000000000000000, 0.000000000000000000, 1.000000000000000000 ) ) ;
#1125 = EDGE_CURVE ( 'NONE', #447, #4102, #18800, .T. ) ;
#1126 = FACE_OUTER_BOUND ( 'NONE', #18409, .T. ) ;
#1127 = B_SPLINE_CURVE_WITH_KNOTS ( 'NONE', 3,
 ( #12933, #14369, #15901, #1274, #17333, #10842, #6356, #7503, #7699, #12086 ),
 .UNSPECIFIED., .F., .F.,
 ( 4, 3, 3, 4 ),
 ( 0.0004168119862255878537, 0.0004599608082120251176, 0.0006467586077648016917, 0.0008336169836825990491 ),
 .UNSPECIFIED. ) ;
#1128 = CARTESIAN_POINT ( 'NONE',  ( 2.949999999999999734, 0.000000000000000000, 0.000000000000000000 ) ) ;
#1129 = ORIENTED_EDGE ( 'NONE', *, *, #12774, .F. ) ;
#1130 = CIRCLE ( 'NONE', #17008, 1.000000000000000000 ) ;
#1132 = ORIENTED_EDGE ( 'NONE', *, *, #3811, .T. ) ;
#1131 = CARTESIAN_POINT ( 'NONE',  ( 3.950837973638676281, -1.958075594453890789, 14.41405733518059940 ) ) ;
#1133 = CARTESIAN_POINT ( 'NONE',  ( 16.56872352241294521, 0.001821578298043785094, -0.01027347319884367241 ) ) ;
#1134 = VECTOR ( 'NONE', #3141, 1000.000000000000114 ) ;
#1135 = CARTESIAN_POINT ( 'NONE',  ( 0.8740764193766140666, 14.27348595579769253, 0.8420116711621705718 ) ) ;
#1136 = ADVANCED_FACE ( 'NONE', ( #12314 ), #18869, .F. ) ;
#1137 = VERTEX_POINT ( 'NONE', #12404 ) ;
#1138 = CARTESIAN_POINT ( 'NONE',  ( 0.3137051932979775248, 3.805684345189972895, -13.20008686438101719 ) ) ;
#1139 = CARTESIAN_POINT ( 'NONE',  ( -30.00000000000000355, -12.50000000000000178, -0.5000000000000000000 ) ) ;
#1140 = CARTESIAN_POINT ( 'NONE',  ( 16.56782317627811096, -0.009228812961908680612, 0.003357783021327786360 ) ) ;
#1142 = SURFACE_STYLE_FILL_AREA ( #6542 ) ;
#1141 =( BOUNDED_SURFACE ( )  B_SPLINE_SURFACE ( 3, 1, ( 
 ( #8181, #15158 ),
 ( #5206, #3771 ),
 ( #6462, #9595 ),
 ( #5020, #907 ) ),
 .UNSPECIFIED., .F., .F., .T. ) 
 B_SPLINE_SURFACE_WITH_KNOTS ( ( 4, 4 ),
 ( 2, 2 ),
 ( 0.000000000000000000, 1.000000000000000000 ),
 ( 0.000000000000000000, 1.000000000000000000 ),
 .UNSPECIFIED. ) 
 GEOMETRIC_REPRESENTATION_ITEM ( )  RATIONAL_B_SPLINE_SURFACE ( (
 ( 1.000000000000000000, 1.000000000000000000),
 ( 0.9593108457356467333, 0.9995965569486454649),
 ( 0.9593108457356467333, 0.9995965569486454649),
 ( 1.000000000000000000, 1.000000000000000000) ) ) 
 REPRESENTATION_ITEM ( '' )  SURFACE ( )  );
#1143 = EDGE_LOOP ( 'NONE', ( #3747, #14066, #8797, #9515 ) ) ;
#1144 = CARTESIAN_POINT ( 'NONE',  ( 2.002547531651519996, 0.6781519942173496185, -12.57989064830758785 ) ) ;
#1145 = AXIS2_PLACEMENT_3D ( 'NONE', #3509, #15177, #651 ) ;
#1146 = ADVANCED_FACE ( 'NONE', ( #16985 ), #12295, .F. ) ;
#1147 = CARTESIAN_POINT ( 'NONE',  ( 3.950837973638668288, 0.000000000000000000, 0.000000000000000000 ) ) ;
#1148 = CARTESIAN_POINT ( 'NONE',  ( 3.950837973638676281, -10.05648675950133963, 10.51028938476214059 ) ) ;
#1149 = CARTESIAN_POINT ( 'NONE',  ( 7.000000000000000000, 0.000000000000000000, -12.00000000000000000 ) ) ;
#1150 = LINE ( 'NONE', #9834, #4116 ) ;
#1151 = SURFACE_STYLE_FILL_AREA ( #9565 ) ;
#1152 = CARTESIAN_POINT ( 'NONE',  ( 1.342453679581834924, -14.34050741580204402, -3.649820028552883233 ) ) ;
#1153 = CARTESIAN_POINT ( 'NONE',  ( 2.747332970342022840, 2.705255688517843371, 16.12459247543627683 ) ) ;
#1155 = ORIENTED_EDGE ( 'NONE', *, *, #5662, .F. ) ;
#1154 = CARTESIAN_POINT ( 'NONE',  ( 8.522092701127531811, -6.489356537178172957, -2.505958102592690473 ) ) ;
#1156 = FACE_OUTER_BOUND ( 'NONE', #9724, .T. ) ;
#1157 = TOROIDAL_SURFACE ( 'NONE', #15806, 2.700000000000000178, 0.2000000000000000111 ) ;
#1158 = DIRECTION ( 'NONE',  ( -1.000000000000000000, 0.000000000000000000, 0.000000000000000000 ) ) ;
#1159 = B_SPLINE_CURVE_WITH_KNOTS ( 'NONE', 3,
 ( #17224, #15420, #1075, #12739, #5471, #11318 ),
 .UNSPECIFIED., .F., .F.,
 ( 4, 2, 4 ),
 ( 3.144186300207962859E-18, 0.0002017457492448081777, 0.0004034914984896132112 ),
 .UNSPECIFIED. ) ;
#1160 = EDGE_CURVE ( 'NONE', #17471, #3540, #11075, .T. ) ;
#1161 = ORIENTED_EDGE ( 'NONE', *, *, #10654, .F. ) ;
#1162 = CARTESIAN_POINT ( 'NONE',  ( 16.56782317627811096, -0.002708056627498708728, -0.009439921864426879458 ) ) ;
#1163 = CARTESIAN_POINT ( 'NONE',  ( 3.950837973638677170, -14.31366178983255466, 2.591948120961746760 ) ) ;
#1164 = CIRCLE ( 'NONE', #7602, 5.000000000000004441 ) ;
#1165 = ORIENTED_EDGE ( 'NONE', *, *, #14548, .F. ) ;
#1166 = CARTESIAN_POINT ( 'NONE',  ( 0.3151928476913582466, 4.245853234426384404, 13.06671852871090778 ) ) ;
#1167 = CARTESIAN_POINT ( 'NONE',  ( 2.747332970342022840, 2.409922051470906990, -16.17136872824896443 ) ) ;
#1168 = CARTESIAN_POINT ( 'NONE',  ( 0.3939822652208163078, 3.598529276937260324, 13.34132036472938410 ) ) ;
#1169 = CARTESIAN_POINT ( 'NONE',  ( -194.9999999999999716, -10.00000000000002665, 11.00000000000000000 ) ) ;
#1170 = CARTESIAN_POINT ( 'NONE',  ( 11.50000000000000178, 0.000000000000000000, 11.00000000000000000 ) ) ;
#1171 = UNCERTAINTY_MEASURE_WITH_UNIT (LENGTH_MEASURE( 1.000000000000000082E-05 ), #17826, 'distance_accuracy_value', 'NONE');
#1172 = EDGE_LOOP ( 'NONE', ( #11818, #17072 ) ) ;
#1173 = ITEM_DEFINED_TRANSFORMATION ( 'NONE', 'NONE', #18813,  #2030 ) ;
#1174 = B_SPLINE_CURVE_WITH_KNOTS ( 'NONE', 3,
 ( #3759, #15417, #2322, #8170, #891, #6734, #12545, #11678, #17127, #10052, #18740, #17412, #15971 ),
 .UNSPECIFIED., .F., .F.,
 ( 4, 3, 3, 3, 4 ),
 ( 2.453269466693398698E-18, 0.0002299804304191474167, 0.0004599608082120242502, 0.0006467586077648022338, 0.0008336169836825977481 ),
 .UNSPECIFIED. ) ;
#1175 = DIRECTION ( 'NONE',  ( 1.540743955509788340E-33, 1.000000000000000000, 2.533398541561209262E-17 ) ) ;
#1176 = CARTESIAN_POINT ( 'NONE',  ( 3.950837973638676281, 1.958075594453990487, -14.41405733518058341 ) ) ;
#1177 =( BOUNDED_SURFACE ( )  B_SPLINE_SURFACE ( 3, 1, ( 
 ( #11687, #4623 ),
 ( #6057, #1855 ),
 ( #2975, #11885 ),
 ( #4531, #13026 ) ),
 .UNSPECIFIED., .F., .F., .T. ) 
 B_SPLINE_SURFACE_WITH_KNOTS ( ( 4, 4 ),
 ( 2, 2 ),
 ( 0.000000000000000000, 1.000000000000000000 ),
 ( 0.000000000000000000, 1.000000000000000000 ),
 .UNSPECIFIED. ) 
 GEOMETRIC_REPRESENTATION_ITEM ( )  RATIONAL_B_SPLINE_SURFACE ( (
 ( 1.000000000000000000, 1.000000000000000000),
 ( 0.9593108457356467333, 0.9995965569486454649),
 ( 0.9593108457356467333, 0.9995965569486454649),
 ( 1.000000000000000000, 1.000000000000000000) ) ) 
 REPRESENTATION_ITEM ( '' )  SURFACE ( )  );
#1178 =( BOUNDED_SURFACE ( )  B_SPLINE_SURFACE ( 3, 1, ( 
 ( #14213, #2533 ),
 ( #8736, #17731 ),
 ( #37, #13319 ),
 ( #1476, #8382 ) ),
 .UNSPECIFIED., .F., .F., .T. ) 
 B_SPLINE_SURFACE_WITH_KNOTS ( ( 4, 4 ),
 ( 2, 2 ),
 ( 0.000000000000000000, 1.000000000000000000 ),
 ( 0.000000000000000000, 1.000000000000000000 ),
 .UNSPECIFIED. ) 
 GEOMETRIC_REPRESENTATION_ITEM ( )  RATIONAL_B_SPLINE_SURFACE ( (
 ( 1.000000000000000000, 1.000000000000000000),
 ( 0.9933953342250436691, 0.8357391271907733676),
 ( 0.9933953342250436691, 0.8357391271907733676),
 ( 1.000000000000000000, 1.000000000000000000) ) ) 
 REPRESENTATION_ITEM ( '' )  SURFACE ( )  );
#1179 = CARTESIAN_POINT ( 'NONE',  ( -20.00000000000000000, -7.500000000000000888, -12.00000000000000000 ) ) ;
#1180 = DIRECTION ( 'NONE',  ( 0.000000000000000000, 0.000000000000000000, 1.000000000000000000 ) ) ;
#1181 = DIRECTION ( 'NONE',  ( -0.000000000000000000, -0.000000000000000000, -1.000000000000000000 ) ) ;
#1182 = VERTEX_POINT ( 'NONE', #2186 ) ;
#1183 = CARTESIAN_POINT ( 'NONE',  ( 16.56782317627811096, 0.007739510688078436902, -0.006045301465876656150 ) ) ;
#1184 = VERTEX_POINT ( 'NONE', #8204 ) ;
#1185 = EDGE_CURVE ( 'NONE', #17332, #1103, #11737, .T. ) ;
#1186 = EDGE_CURVE ( 'NONE', #5607, #14673, #5331, .T. ) ;
#1187 = VERTEX_POINT ( 'NONE', #2444 ) ;
#1188 = ORIENTED_EDGE ( 'NONE', *, *, #2248, .T. ) ;
#1189 = DIRECTION ( 'NONE',  ( -1.000000000000000000, -0.000000000000000000, -0.000000000000000000 ) ) ;
#1190 = ORIENTED_EDGE ( 'NONE', *, *, #7855, .T. ) ;
#1191 = CARTESIAN_POINT ( 'NONE',  ( 1.846138399168762101, 12.43476674860266584, -0.4167076046095982700 ) ) ;
#1192 = CARTESIAN_POINT ( 'NONE',  ( 0.000000000000000000, 0.000000000000000000, 2.500000000000000000 ) ) ;
#1193 = CARTESIAN_POINT ( 'NONE',  ( 0.3058872367615226295, 4.821066432589507400, -12.87003593440623206 ) ) ;
#1194 = DIRECTION ( 'NONE',  ( -0.000000000000000000, -0.000000000000000000, -1.000000000000000000 ) ) ;
#1195 = CARTESIAN_POINT ( 'NONE',  ( 20.00000000000000000, 2.499999999999998668, -16.99999999999999645 ) ) ;
#1196 = CARTESIAN_POINT ( 'NONE',  ( 8.438534575730034959, 5.415535776177581972, -4.221456476902606170 ) ) ;
#1197 = VECTOR ( 'NONE', #8771, 1000.000000000000114 ) ;
#1198 = CARTESIAN_POINT ( 'NONE',  ( 16.56872352241294521, 0.009207754980063749192, 0.004907101719994666836 ) ) ;
#1199 = CARTESIAN_POINT ( 'NONE',  ( 1.499999999999999112, 4.769696007084728073, 5.000000000000000000 ) ) ;
#1200 = ORIENTED_EDGE ( 'NONE', *, *, #12873, .F. ) ;
#1201 = ORIENTED_EDGE ( 'NONE', *, *, #10324, .F. ) ;
#1202 =( GEOMETRIC_REPRESENTATION_CONTEXT ( 3 ) GLOBAL_UNCERTAINTY_ASSIGNED_CONTEXT ( ( #1171 ) ) GLOBAL_UNIT_ASSIGNED_CONTEXT ( ( #17826, #3665, #10559 ) ) REPRESENTATION_CONTEXT ( 'NONE', 'WORKASPACE' ) );
#1203 = ORIENTED_EDGE ( 'NONE', *, *, #13767, .T. ) ;
#1204 = EDGE_LOOP ( 'NONE', ( #8182, #16614, #818 ) ) ;
#1205 = DIRECTION ( 'NONE',  ( -0.9034263296138843602, 0.000000000000000000, -0.4287433579198459133 ) ) ;
#1206 = EDGE_CURVE ( 'NONE', #11439, #12620, #9798, .T. ) ;
#1207 = FACE_OUTER_BOUND ( 'NONE', #3846, .T. ) ;
#1208 = ORIENTED_EDGE ( 'NONE', *, *, #16911, .F. ) ;
#1209 = CYLINDRICAL_SURFACE ( 'NONE', #766, 5.000000000000000888 ) ;
#1210 = DIRECTION ( 'NONE',  ( -1.000000000000000000, -0.000000000000000000, -0.000000000000000000 ) ) ;
#1211 = CARTESIAN_POINT ( 'NONE',  ( 1.517261107235507778, 6.836011689345040665, -11.99999999467225997 ) ) ;
#1212 = CARTESIAN_POINT ( 'NONE',  ( 0.3148213771069364175, -11.24846294176317407, 7.888490156175182122 ) ) ;
#1213 = ADVANCED_FACE ( 'NONE', ( #18685 ), #14306, .T. ) ;
#1214 = DIRECTION ( 'NONE',  ( -1.000000000000000000, -0.000000000000000000, -0.000000000000000000 ) ) ;
#1215 = FACE_OUTER_BOUND ( 'NONE', #8044, .T. ) ;
#1216 = CARTESIAN_POINT ( 'NONE',  ( -4.505465888036630062, -19.31487138727242581, 6.000000000000000000 ) ) ;
#1217 = CARTESIAN_POINT ( 'NONE',  ( 0.3137051932979792457, 4.679953077377485116, 12.91601973349272114 ) ) ;
#1218 = ORIENTED_EDGE ( 'NONE', *, *, #2619, .T. ) ;
#1219 = ORIENTED_EDGE ( 'NONE', *, *, #192, .T. ) ;
#1220 = CARTESIAN_POINT ( 'NONE',  ( 1.342453679581834924, 11.38190519890867236, -9.456403821038676938 ) ) ;
#1221 = CIRCLE ( 'NONE', #2701, 1.000000000000000000 ) ;
#1222 = ORIENTED_EDGE ( 'NONE', *, *, #14362, .F. ) ;
#1223 = ORIENTED_EDGE ( 'NONE', *, *, #12186, .F. ) ;
#1224 = ADVANCED_FACE ( 'NONE', ( #6855 ), #12955, .F. ) ;
#1225 = CARTESIAN_POINT ( 'NONE',  ( 16.56872352241294521, 0.01027347319884366721, 0.001821578298043820656 ) ) ;
#1226 = EDGE_LOOP ( 'NONE', ( #3328, #17393 ) ) ;
#1227 = DIRECTION ( 'NONE',  ( 0.000000000000000000, 0.000000000000000000, -1.000000000000000000 ) ) ;
#1228 = B_SPLINE_CURVE_WITH_KNOTS ( 'NONE', 3,
 ( #4633, #4434, #7410, #16296 ),
 .UNSPECIFIED., .F., .F.,
 ( 4, 4 ),
 ( 2.211347213673310975E-17, 0.003005512676784851799 ),
 .UNSPECIFIED. ) ;
#1229 = ADVANCED_FACE ( 'NONE', ( #14392 ), #17355, .T. ) ;
#1230 = EDGE_CURVE ( 'NONE', #18002, #13478, #8565, .T. ) ;
#1231 = CARTESIAN_POINT ( 'NONE',  ( 1.846955891736115740, -12.44001089941741967, 0.2634721419534765685 ) ) ;
#1232 = DIRECTION ( 'NONE',  ( 0.000000000000000000, 0.000000000000000000, 1.000000000000000000 ) ) ;
#1233 = CARTESIAN_POINT ( 'NONE',  ( 1.846955891736116184, -0.2634721419534329923, -12.44001089941741611 ) ) ;
#1234 = ORIENTED_EDGE ( 'NONE', *, *, #4931, .F. ) ;
#1235 = CARTESIAN_POINT ( 'NONE',  ( 2.697797270744668019, 7.053988368581864066, 11.26906156738829168 ) ) ;
#1236 = DIRECTION ( 'NONE',  ( 0.7071067818211358436, 8.659560554583467185E-17, 0.7071067805519591909 ) ) ;
#1237 = DIRECTION ( 'NONE',  ( 0.000000000000000000, 0.000000000000000000, -1.000000000000000000 ) ) ;
#1238 = DIRECTION ( 'NONE',  ( -0.000000000000000000, -0.000000000000000000, 1.000000000000000000 ) ) ;
#1239 = CARTESIAN_POINT ( 'NONE',  ( 0.4385251269669960816, -8.732456510146150208, 10.76637725024249193 ) ) ;
#1240 = ADVANCED_BREP_SHAPE_REPRESENTATION ( '', ( #9885, #2030 ), #4780 ) ;
#1241 = EDGE_CURVE ( 'NONE', #18187, #18838, #13054, .T. ) ;
#1242 = CARTESIAN_POINT ( 'NONE',  ( 2.636624412716913390, 14.14563173255587536, -7.605649742760633991 ) ) ;
#1243 = CIRCLE ( 'NONE', #11940, 2.600000000000039613 ) ;
#1244 = DIRECTION ( 'NONE',  ( 0.000000000000000000, 0.000000000000000000, 1.000000000000000000 ) ) ;
#1246 = ORIENTED_EDGE ( 'NONE', *, *, #1941, .F. ) ;
#1245 = DIRECTION ( 'NONE',  ( 0.000000000000000000, 0.000000000000000000, 1.000000000000000000 ) ) ;
#1247 = CARTESIAN_POINT ( 'NONE',  ( 2.123976203522053741, -6.261444813538457943, -14.31368049382976260 ) ) ;
#1248 = CARTESIAN_POINT ( 'NONE',  ( 1.560000000000000053, 1.732050807568878747, 7.017607234860990640E-28 ) ) ;
#1249 =( BOUNDED_SURFACE ( )  B_SPLINE_SURFACE ( 3, 1, ( 
 ( #12346, #18183 ),
 ( #3653, #9484 ),
 ( #12809, #967 ),
 ( #877, #8418 ) ),
 .UNSPECIFIED., .F., .F., .T. ) 
 B_SPLINE_SURFACE_WITH_KNOTS ( ( 4, 4 ),
 ( 2, 2 ),
 ( 0.000000000000000000, 1.000000000000000000 ),
 ( 0.000000000000000000, 1.000000000000000000 ),
 .UNSPECIFIED. ) 
 GEOMETRIC_REPRESENTATION_ITEM ( )  RATIONAL_B_SPLINE_SURFACE ( (
 ( 1.000000000000000000, 1.000000000000000000),
 ( 0.9933953342250438912, 0.8357391271907739227),
 ( 0.9933953342250438912, 0.8357391271907739227),
 ( 1.000000000000000000, 1.000000000000000000) ) ) 
 REPRESENTATION_ITEM ( '' )  SURFACE ( )  );
#1250 = ORIENTED_EDGE ( 'NONE', *, *, #18133, .T. ) ;
#1251 = CARTESIAN_POINT ( 'NONE',  ( 1.846138399168762989, 9.815003036200414144, 7.646096044339929954 ) ) ;
#1252 = CARTESIAN_POINT ( 'NONE',  ( 1.254009781011992342, -5.487405433548717681, -13.61532727684465982 ) ) ;
#1253 = EDGE_LOOP ( 'NONE', ( #18351, #12029, #16983, #6300 ) ) ;
#1254 = CARTESIAN_POINT ( 'NONE',  ( 20.00000000000000711, -24.99999999999999645, 6.000000000000000000 ) ) ;
#1255 = FACE_OUTER_BOUND ( 'NONE', #3235, .T. ) ;
#1256 = B_SPLINE_CURVE_WITH_KNOTS ( 'NONE', 3,
 ( #12154, #13570, #6696, #3342, #6507, #17982, #16732, #15105, #8043, #3633, #2021, #9468, #7860 ),
 .UNSPECIFIED., .F., .F.,
 ( 4, 3, 3, 3, 4 ),
 ( 1.734723475976806902E-18, 0.0002299804304191488261, 0.0004599608082120263644, 0.0006467586077648019086, 0.0008336169836826000249 ),
 .UNSPECIFIED. ) ;
#1257 = VECTOR ( 'NONE', #4220, 1000.000000000000000 ) ;
#1258 = CARTESIAN_POINT ( 'NONE',  ( 0.3939875929385667219, -3.598491969338320384, 13.34133634968953785 ) ) ;
#1259 = CARTESIAN_POINT ( 'NONE',  ( 0.3142011359265332593, -10.88514493056448096, 8.382042760265870029 ) ) ;
#1260 = CARTESIAN_POINT ( 'NONE',  ( 2.636624412716062960, 6.973567714909310489, -14.46769361191320868 ) ) ;
#1261 = ORIENTED_EDGE ( 'NONE', *, *, #6767, .F. ) ;
#1262 = EDGE_CURVE ( 'NONE', #7136, #7670, #2721, .T. ) ;
#1263 = CARTESIAN_POINT ( 'NONE',  ( -194.9999999999999716, 9.999999999999973355, 3.000000000000000000 ) ) ;
#1264 = EDGE_CURVE ( 'NONE', #3, #15917, #15366, .T. ) ;
#1265 = CARTESIAN_POINT ( 'NONE',  ( -11.50000000000000178, 1.438959988998140357E-15, 10.00000000000000000 ) ) ;
#1266 = CARTESIAN_POINT ( 'NONE',  ( 0.3307726912345213544, -10.76786801061213161, 8.558645027434234720 ) ) ;
#1267 = DIRECTION ( 'NONE',  ( -0.000000000000000000, -0.000000000000000000, 1.000000000000000000 ) ) ;
#1268 = CARTESIAN_POINT ( 'NONE',  ( 20.00000000000000000, -7.500000000000000888, -17.00000000000000000 ) ) ;
#1269 = ORIENTED_EDGE ( 'NONE', *, *, #10296, .F. ) ;
#1270 = DIRECTION ( 'NONE',  ( -1.000000000000000000, -0.000000000000000000, -0.000000000000000000 ) ) ;
#1271 = FACE_OUTER_BOUND ( 'NONE', #2673, .T. ) ;
#1272 = ORIENTED_EDGE ( 'NONE', *, *, #5435, .F. ) ;
#1273 = ORIENTED_EDGE ( 'NONE', *, *, #546, .F. ) ;
#1274 = CARTESIAN_POINT ( 'NONE',  ( 1.847412631396504246, -0.04315047898443813423, 12.44294644888238999 ) ) ;
#1275 = ORIENTED_EDGE ( 'NONE', *, *, #909, .T. ) ;
#1276 = CARTESIAN_POINT ( 'NONE',  ( 0.3095370825347234511, 4.681152801286343923, -12.91933430393602933 ) ) ;
#1277 = AXIS2_PLACEMENT_3D ( 'NONE', #16062, #13389, #11959 ) ;
#1278 = ORIENTED_EDGE ( 'NONE', *, *, #18035, .T. ) ;
#1279 = CARTESIAN_POINT ( 'NONE',  ( 1.846138399168762101, 12.43476674860266584, -0.4167076046095982700 ) ) ;
#1280 = CYLINDRICAL_SURFACE ( 'NONE', #14175, 5.000000000000000000 ) ;
#1281 = FACE_OUTER_BOUND ( 'NONE', #599, .T. ) ;
#1283 = CARTESIAN_POINT ( 'NONE',  ( 0.3095370825347224519, 0.4597470195092092093, -13.73357284481724250 ) ) ;
#1282 =( BOUNDED_SURFACE ( )  B_SPLINE_SURFACE ( 3, 1, ( 
 ( #12044, #16349 ),
 ( #3332, #3229 ),
 ( #17584, #17484 ),
 ( #16048, #10322 ) ),
 .UNSPECIFIED., .F., .F., .T. ) 
 B_SPLINE_SURFACE_WITH_KNOTS ( ( 4, 4 ),
 ( 2, 2 ),
 ( 0.000000000000000000, 1.000000000000000000 ),
 ( 0.000000000000000000, 1.000000000000000000 ),
 .UNSPECIFIED. ) 
 GEOMETRIC_REPRESENTATION_ITEM ( )  RATIONAL_B_SPLINE_SURFACE ( (
 ( 1.000000000000000000, 1.000000000000000000),
 ( 0.7792777138730158093, 0.9689936506012928330),
 ( 0.7792777138730158093, 0.9689936506012928330),
 ( 1.000000000000000000, 1.000000000000000000) ) ) 
 REPRESENTATION_ITEM ( '' )  SURFACE ( )  );
#1284 =( BOUNDED_SURFACE ( )  B_SPLINE_SURFACE ( 3, 1, ( 
 ( #2638, #16020 ),
 ( #14586, #4367 ),
 ( #15833, #11356 ),
 ( #14396, #10192 ) ),
 .UNSPECIFIED., .F., .F., .T. ) 
 B_SPLINE_SURFACE_WITH_KNOTS ( ( 4, 4 ),
 ( 2, 2 ),
 ( 0.000000000000000000, 1.000000000000000000 ),
 ( 0.000000000000000000, 1.000000000000000000 ),
 .UNSPECIFIED. ) 
 GEOMETRIC_REPRESENTATION_ITEM ( )  RATIONAL_B_SPLINE_SURFACE ( (
 ( 1.000000000000000000, 1.000000000000000000),
 ( 0.7792777138730160313, 0.9689936506012927220),
 ( 0.7792777138730160313, 0.9689936506012927220),
 ( 1.000000000000000000, 1.000000000000000000) ) ) 
 REPRESENTATION_ITEM ( '' )  SURFACE ( )  );
#1285 = EDGE_CURVE ( 'NONE', #10015, #2548, #5780, .T. ) ;
#1286 = ADVANCED_FACE ( 'NONE', ( #11626 ), #2628, .T. ) ;
#1287 = DIRECTION ( 'NONE',  ( -1.000000000000000000, -0.000000000000000000, -0.000000000000000000 ) ) ;
#1288 = ADVANCED_FACE ( 'NONE', ( #11347 ), #1322, .F. ) ;
#1289 = LINE ( 'NONE', #9710, #13681 ) ;
#1290 = AXIS2_PLACEMENT_3D ( 'NONE', #1861, #1565, #7701 ) ;
#1291 = CARTESIAN_POINT ( 'NONE',  ( 16.56822296793089322, 0.009385634690641620620, 0.003834730849370876320 ) ) ;
#1292 = CARTESIAN_POINT ( 'NONE',  ( -1.500000000000001332, 6.799999999999999822, 7.000000000000000000 ) ) ;
#1293 = VERTEX_POINT ( 'NONE', #2810 ) ;
#1294 = ORIENTED_EDGE ( 'NONE', *, *, #5885, .F. ) ;
#1295 = VECTOR ( 'NONE', #18044, 1000.000000000000114 ) ;
#1296 = ORIENTED_EDGE ( 'NONE', *, *, #18671, .F. ) ;
#1297 = ORIENTED_EDGE ( 'NONE', *, *, #5077, .T. ) ;
#1298 = ORIENTED_EDGE ( 'NONE', *, *, #13046, .T. ) ;
#1299 = CARTESIAN_POINT ( 'NONE',  ( 20.00000000000000000, 2.499999999999998668, -16.99999999999999645 ) ) ;
#1300 = CARTESIAN_POINT ( 'NONE',  ( 16.56679352167444819, -0.009170718284672552470, -0.001518074900130618379 ) ) ;
#1301 = CARTESIAN_POINT ( 'NONE',  ( -61.35602477868049220, 9.999999999999973355, 6.000000000000000000 ) ) ;
#1302 = VERTEX_POINT ( 'NONE', #9898 ) ;
#1303 = CARTESIAN_POINT ( 'NONE',  ( 0.3095370825347233956, -8.444334731363927204, -10.84046130709067590 ) ) ;
#1304 = CARTESIAN_POINT ( 'NONE',  ( 3.950837973638668288, 0.000000000000000000, 0.000000000000000000 ) ) ;
#1305 = CARTESIAN_POINT ( 'NONE',  ( 1.870513085853429791, 6.747912118474282295, -12.00000000532774003 ) ) ;
#1306 = CARTESIAN_POINT ( 'NONE',  ( 2.002547531651519996, -12.17374746633580784, 3.242439124566603326 ) ) ;
#1307 = EDGE_CURVE ( 'NONE', #11625, #16657, #17189, .T. ) ;
#1308 = AXIS2_PLACEMENT_3D ( 'NONE', #10783, #18228, #8012 ) ;
#1309 = DIRECTION ( 'NONE',  ( 1.000000000000000000, 0.000000000000000000, 0.000000000000000000 ) ) ;
#1310 = CARTESIAN_POINT ( 'NONE',  ( -194.9999999999999716, -25.00000000000003197, 0.000000000000000000 ) ) ;
#1311 = CARTESIAN_POINT ( 'NONE',  ( -61.35602477868047799, -10.00000000000000888, -153.7432847437423789 ) ) ;
#1312 = EDGE_CURVE ( 'NONE', #1583, #8583, #4177, .T. ) ;
#1313 = DIRECTION ( 'NONE',  ( 0.000000000000000000, 0.000000000000000000, 1.000000000000000000 ) ) ;
#1314 = ORIENTED_EDGE ( 'NONE', *, *, #723, .T. ) ;
#1315 = EDGE_CURVE ( 'NONE', #12766, #16531, #8955, .T. ) ;
#1316 = ORIENTED_EDGE ( 'NONE', *, *, #6908, .T. ) ;
#1317 = CYLINDRICAL_SURFACE ( 'NONE', #216, 5.000000000000000000 ) ;
#1318 = ORIENTED_EDGE ( 'NONE', *, *, #5137, .T. ) ;
#1319 = VERTEX_POINT ( 'NONE', #5985 ) ;
#1320 = CARTESIAN_POINT ( 'NONE',  ( 1.342453679581834924, 5.476372339890209773, -13.74702459364878315 ) ) ;
#1321 = AXIS2_PLACEMENT_3D ( 'NONE', #17112, #8244, #5361 ) ;
#1322 = TOROIDAL_SURFACE ( 'NONE', #12022, 2.699999999999999734, 0.2000000000000000111 ) ;
#1323 = EDGE_LOOP ( 'NONE', ( #2426, #4863, #8855, #15183 ) ) ;
#1324 = CARTESIAN_POINT ( 'NONE',  ( 2.636624412715384391, -11.60464335004044223, -11.10302021258006278 ) ) ;
#1325 = CARTESIAN_POINT ( 'NONE',  ( 1.254255976357644409, -12.44256109021810097, 7.789651112956895496 ) ) ;
#1326 = CARTESIAN_POINT ( 'NONE',  ( -54.57590088527786065, 9.999999999999973355, 6.000000000000000000 ) ) ;
#1327 = CARTESIAN_POINT ( 'NONE',  ( 1.321128355694181398E-14, -7.013167318348350499, 25.01316734529530095 ) ) ;
#1328 = ORIENTED_EDGE ( 'NONE', *, *, #14692, .F. ) ;
#1329 = DIRECTION ( 'NONE',  ( 0.000000000000000000, -0.000000000000000000, 1.000000000000000000 ) ) ;
#1330 = CARTESIAN_POINT ( 'NONE',  ( 1.959283090834841090, -10.53516775895155000, -6.829027319138364582 ) ) ;
#1331 = CARTESIAN_POINT ( 'NONE',  ( 1.847168016377980670, 12.44137401948661470, -0.1868244120189998803 ) ) ;
#1332 = DIRECTION ( 'NONE',  ( 0.000000000000000000, 0.000000000000000000, 1.000000000000000000 ) ) ;
#1333 = DIRECTION ( 'NONE',  ( -1.000000000000000000, -0.000000000000000000, -0.000000000000000000 ) ) ;
#1334 = CARTESIAN_POINT ( 'NONE',  ( 1.298018465182615993E-15, -10.00000000000000000, -2.000000000000000000 ) ) ;
#1335 = CARTESIAN_POINT ( 'NONE',  ( 0.000000000000000000, 0.000000000000000000, 0.000000000000000000 ) ) ;
#1336 = FACE_OUTER_BOUND ( 'NONE', #12011, .T. ) ;
#1337 = ORIENTED_EDGE ( 'NONE', *, *, #2143, .F. ) ;
#1338 = VECTOR ( 'NONE', #7072, 1000.000000000000114 ) ;
#1339 = CIRCLE ( 'NONE', #6236, 16.06066017081991149 ) ;
#1340 = EDGE_CURVE ( 'NONE', #14073, #3822, #9891, .T. ) ;
#1341 = DIRECTION ( 'NONE',  ( 0.000000000000000000, 0.000000000000000000, 1.000000000000000000 ) ) ;
#1343 = VERTEX_POINT ( 'NONE', #6085 ) ;
#1342 = DIRECTION ( 'NONE',  ( 0.000000000000000000, 0.000000000000000000, 1.000000000000000000 ) ) ;
#1344 = CARTESIAN_POINT ( 'NONE',  ( 16.56872352241294521, -0.009382111268606286789, 0.004564908236400187953 ) ) ;
#1345 = CARTESIAN_POINT ( 'NONE',  ( 2.369999999999999662, 4.749999999999999112, 0.000000000000000000 ) ) ;
#1346 = ORIENTED_EDGE ( 'NONE', *, *, #6444, .T. ) ;
#1347 = CARTESIAN_POINT ( 'NONE',  ( 0.3720661004400037664, -4.951033743989731839, 12.89739157014191129 ) ) ;
#1348 = CARTESIAN_POINT ( 'NONE',  ( 1.846138399168762101, 12.43476674860266584, -0.4167076046095982700 ) ) ;
#1349 = ORIENTED_EDGE ( 'NONE', *, *, #7948, .T. ) ;
#1350 = CARTESIAN_POINT ( 'NONE',  ( 0.000000000000000000, 0.000000000000000000, -3.000000000000000000 ) ) ;
#1351 = CARTESIAN_POINT ( 'NONE',  ( 2.747332970342022840, -7.555624153089539163, -14.49942876448600693 ) ) ;
#1352 = B_SPLINE_CURVE_WITH_KNOTS ( 'NONE', 3,
 ( #13112, #3152, #9003, #17609, #14830, #18 ),
 .UNSPECIFIED., .F., .F.,
 ( 4, 2, 4 ),
 ( 2.017461075144244397E-18, 0.0002017457492448097769, 0.0004034914984896175480 ),
 .UNSPECIFIED. ) ;
#1353 = ADVANCED_FACE ( 'NONE', ( #1587 ), #8852, .F. ) ;
#1354 = CARTESIAN_POINT ( 'NONE',  ( 8.522092701127531811, 5.841710761610186431, -3.777034505568459100 ) ) ;
#1355 = CARTESIAN_POINT ( 'NONE',  ( 0.000000000000000000, 0.000000000000000000, 6.000000000000000000 ) ) ;
#1356 = CARTESIAN_POINT ( 'NONE',  ( 0.000000000000000000, 0.000000000000000000, 3.000000000000000000 ) ) ;
#1357 = ORIENTED_EDGE ( 'NONE', *, *, #7230, .T. ) ;
#1358 = VECTOR ( 'NONE', #13265, 1000.000000000000000 ) ;
#1359 = CONTEXT_DEPENDENT_SHAPE_REPRESENTATION ( #10111, #10431 ) ;
#1360 = DIRECTION ( 'NONE',  ( -1.000000000000000000, -0.000000000000000000, -0.000000000000000000 ) ) ;
#1361 = CARTESIAN_POINT ( 'NONE',  ( 2.697797270744668019, -12.89731672021093090, 3.226410068829379973 ) ) ;
#1362 =( BOUNDED_SURFACE ( )  B_SPLINE_SURFACE ( 3, 1, ( 
 ( #11523, #11804 ),
 ( #17639, #10466 ),
 ( #16301, #7125 ),
 ( #17342, #4259 ) ),
 .UNSPECIFIED., .F., .F., .T. ) 
 B_SPLINE_SURFACE_WITH_KNOTS ( ( 4, 4 ),
 ( 2, 2 ),
 ( 0.000000000000000000, 1.000000000000000000 ),
 ( 0.000000000000000000, 1.000000000000000000 ),
 .UNSPECIFIED. ) 
 GEOMETRIC_REPRESENTATION_ITEM ( )  RATIONAL_B_SPLINE_SURFACE ( (
 ( 1.000000000000000000, 1.000000000000000000),
 ( 0.9933953342250438912, 0.8357391271907739227),
 ( 0.9933953342250438912, 0.8357391271907739227),
 ( 1.000000000000000000, 1.000000000000000000) ) ) 
 REPRESENTATION_ITEM ( '' )  SURFACE ( )  );
#1363 = CARTESIAN_POINT ( 'NONE',  ( 0.3137051932979792457, 0.4596302728641686874, -13.73004976592201487 ) ) ;
#1364 = CARTESIAN_POINT ( 'NONE',  ( 3.512766787570723803, -13.25664064834472100, -7.127386085302978458 ) ) ;
#1365 = CARTESIAN_POINT ( 'NONE',  ( 2.750000000000000000, 2.499999999999999112, 0.000000000000000000 ) ) ;
#1366 = VECTOR ( 'NONE', #18178, 1000.000000000000000 ) ;
#1367 = ORIENTED_EDGE ( 'NONE', *, *, #11992, .F. ) ;
#1368 = DIRECTION ( 'NONE',  ( 1.000000000000000000, -0.000000000000000000, -0.000000000000000000 ) ) ;
#1369 = VECTOR ( 'NONE', #13910, 1000.000000000000000 ) ;
#1370 = VERTEX_POINT ( 'NONE', #7724 ) ;
#1371 = AXIS2_PLACEMENT_3D ( 'NONE', #17480, #5906, #4386 ) ;
#1372 = EDGE_CURVE ( 'NONE', #1703, #15433, #2903, .T. ) ;
#1373 = ORIENTED_EDGE ( 'NONE', *, *, #18131, .T. ) ;
#1374 = CARTESIAN_POINT ( 'NONE',  ( 1.254255976357440572, -14.24071337840763363, 3.563435620217590749 ) ) ;
#1375 = VERTEX_POINT ( 'NONE', #16316 ) ;
#1376 = DIRECTION ( 'NONE',  ( 0.7561779333270775005, 0.03481510524965243658, -0.6534392409364818688 ) ) ;
#1377 = VERTEX_POINT ( 'NONE', #7431 ) ;
#1378 = DIRECTION ( 'NONE',  ( 1.000000000000000000, 0.000000000000000000, 0.000000000000000000 ) ) ;
#1379 = DIRECTION ( 'NONE',  ( 0.000000000000000000, 0.000000000000000000, 1.000000000000000000 ) ) ;
#1380 = EDGE_CURVE ( 'NONE', #9425, #7190, #8549, .T. ) ;
#1381 = VECTOR ( 'NONE', #12196, 1000.000000000000000 ) ;
#1382 = FACE_OUTER_BOUND ( 'NONE', #10839, .T. ) ;
#1383 = CARTESIAN_POINT ( 'NONE',  ( 16.56679352167444819, -0.001518074900130714439, 0.009170718284672536857 ) ) ;
#1384 = AXIS2_PLACEMENT_3D ( 'NONE', #11061, #7830, #17957 ) ;
#1385 = SURFACE_SIDE_STYLE ('',( #10081 ) ) ;
#1386 = CARTESIAN_POINT ( 'NONE',  ( 0.3137051932979792457, -3.805684345189695783, -13.20008686438109891 ) ) ;
#1387 = LINE ( 'NONE', #17642, #18551 ) ;
#1388 = CARTESIAN_POINT ( 'NONE',  ( 0.3142011359265348691, -12.94258167753015520, 4.608101617236726177 ) ) ;
#1389 = DIRECTION ( 'NONE',  ( -0.000000000000000000, 0.000000000000000000, -1.000000000000000000 ) ) ;
#1390 = ORIENTED_EDGE ( 'NONE', *, *, #14686, .T. ) ;
#1391 = VERTEX_POINT ( 'NONE', #12012 ) ;
#1392 = ORIENTED_EDGE ( 'NONE', *, *, #8942, .F. ) ;
#1393 = ORIENTED_EDGE ( 'NONE', *, *, #11938, .T. ) ;
#1394 = CIRCLE ( 'NONE', #16957, 3.499999999999992895 ) ;
#1395 = ORIENTED_EDGE ( 'NONE', *, *, #16139, .T. ) ;
#1396 = COLOUR_RGB ( '', 0.66274510, 0.83137255, 0.94901961) ;
#1397 = EDGE_CURVE ( 'NONE', #13310, #10284, #3978, .T. ) ;
#1398 = EDGE_CURVE ( 'NONE', #6394, #15029, #3299, .T. ) ;
#1399 = CARTESIAN_POINT ( 'NONE',  ( 2.636624412714236865, 1.966863607038798701E-15, 16.06066017081991149 ) ) ;
#1400 = CARTESIAN_POINT ( 'NONE',  ( 0.3170788640506440603, 13.74111462631963576, 0.1533108587036622894 ) ) ;
#1401 = CARTESIAN_POINT ( 'NONE',  ( 16.56782317627811096, -0.009814734722107087972, -0.0003415813796005906337 ) ) ;
#1402 = ORIENTED_EDGE ( 'NONE', *, *, #14672, .T. ) ;
#1403 = CARTESIAN_POINT ( 'NONE',  ( 2.636624412714763555, 6.973567714907159321, 14.46769361191226722 ) ) ;
#1404 = CARTESIAN_POINT ( 'NONE',  ( 0.3939875929385629472, 0.7003304234513173521, 13.80036004410494854 ) ) ;
#1405 = CARTESIAN_POINT ( 'NONE',  ( 1.845756295923355328, -3.386818134580144690, 11.97166802574125022 ) ) ;
#1406 = CARTESIAN_POINT ( 'NONE',  ( 3.950837973638675393, 10.51028938476217967, 10.05648675950130233 ) ) ;
#1407 = CARTESIAN_POINT ( 'NONE',  ( 0.000000000000000000, 0.000000000000000000, -13.42403576283810906 ) ) ;
#1408 = CARTESIAN_POINT ( 'NONE',  ( 1.861628059977341598, 12.00316790821106139, -3.332996951203504032 ) ) ;
#1409 = CARTESIAN_POINT ( 'NONE',  ( 2.002547531651519996, -9.778737580845639599, -7.942910686618280813 ) ) ;
#1410 = CARTESIAN_POINT ( 'NONE',  ( 0.4385251269669958596, -12.93791070501030660, -4.978066129061825329 ) ) ;
#1411 = AXIS2_PLACEMENT_3D ( 'NONE', #6939, #15993, #5664 ) ;
#1412 = CARTESIAN_POINT ( 'NONE',  ( 1.846822687350026193, -4.121816957446279517, 11.74004266906802663 ) ) ;
#1413 = ORIENTED_EDGE ( 'NONE', *, *, #12049, .F. ) ;
#1414 = PRODUCT ( 'High-Hardness Steel Cutting Wheel', 'High-Hardness Steel Cutting Wheel', '', ( #12280 ) ) ;
#1415 = ORIENTED_EDGE ( 'NONE', *, *, #1838, .T. ) ;
#1416 = ORIENTED_EDGE ( 'NONE', *, *, #14728, .F. ) ;
#1417 = AXIS2_PLACEMENT_3D ( 'NONE', #8399, #17095, #15747 ) ;
#1418 = ORIENTED_EDGE ( 'NONE', *, *, #13120, .F. ) ;
#1419 = CARTESIAN_POINT ( 'NONE',  ( 4.336808689942014581E-15, -27.00000000000000000, 26.00000000000000000 ) ) ;
#1420 = EDGE_CURVE ( 'NONE', #13478, #12877, #1720, .T. ) ;
#1421 = ORIENTED_EDGE ( 'NONE', *, *, #17693, .F. ) ;
#1422 = ADVANCED_FACE ( 'NONE', ( #8943 ), #728, .T. ) ;
#1423 = EDGE_CURVE ( 'NONE', #16417, #12155, #15163, .T. ) ;
#1424 = CARTESIAN_POINT ( 'NONE',  ( 0.3137051932979792457, -3.805684345189695783, -13.20008686438109891 ) ) ;
#1425 = CARTESIAN_POINT ( 'NONE',  ( 1.846613052777652975, 11.93415846513961753, 3.520031056876344433 ) ) ;
#1426 = DIRECTION ( 'NONE',  ( -0.7635533937278216055, -0.3620487483322522015, 0.5347026451755926280 ) ) ;
#1427 = PRESENTATION_LAYER_ASSIGNMENT (  '', '', ( #9380 ) ) ;
#1428 = LINE ( 'NONE', #1613, #8402 ) ;
#1429 = ORIENTED_EDGE ( 'NONE', *, *, #9598, .F. ) ;
#1430 = CARTESIAN_POINT ( 'NONE',  ( 2.002547531651519996, -9.778737580845639599, -7.942910686618280813 ) ) ;
#1431 = AXIS2_PLACEMENT_3D ( 'NONE', #13888, #9216, #7903 ) ;
#1432 = CARTESIAN_POINT ( 'NONE',  ( -199.9999999999999716, -25.00000000000003197, 3.000000000000000000 ) ) ;
#1433 = B_SPLINE_CURVE_WITH_KNOTS ( 'NONE', 3,
 ( #5635, #11493, #9844, #16943, #14262, #1348 ),
 .UNSPECIFIED., .F., .F.,
 ( 4, 2, 4 ),
 ( 5.421010862427522170E-19, 0.0001825746017570580189, 0.0003651492035141154957 ),
 .UNSPECIFIED. ) ;
#1434 = CARTESIAN_POINT ( 'NONE',  ( 0.3145734862173260593, -13.73540602248380615, -0.3064017202076792512 ) ) ;
#1435 = FACE_OUTER_BOUND ( 'NONE', #7651, .T. ) ;
#1436 = CARTESIAN_POINT ( 'NONE',  ( -194.9999999999999716, -10.00000000000002665, -2.000000000000000000 ) ) ;
#1437 = CARTESIAN_POINT ( 'NONE',  ( 1.846613052777650976, 7.585914669018171352, 9.862487290071024759 ) ) ;
#1438 = AXIS2_PLACEMENT_3D ( 'NONE', #17621, #10448, #16285 ) ;
#1439 = CIRCLE ( 'NONE', #6339, 2.500000000000000000 ) ;
#1440 = CIRCLE ( 'NONE', #17939, 1.000000000000000000 ) ;
#1441 = FACE_OUTER_BOUND ( 'NONE', #12105, .T. ) ;
#1442 = EDGE_LOOP ( 'NONE', ( #18668, #4195, #17241, #11960 ) ) ;
#1443 = CARTESIAN_POINT ( 'NONE',  ( 2.320520222537238553, -13.71278186123262799, 7.743191299717230969 ) ) ;
#1445 = VERTEX_POINT ( 'NONE', #3754 ) ;
#1444 = DIRECTION ( 'NONE',  ( 1.540743955509788340E-33, 1.000000000000000000, 2.533398541561209262E-17 ) ) ;
#1446 = CARTESIAN_POINT ( 'NONE',  ( 0.4754618798421162973, 3.583352865732857495, -13.45049478164055756 ) ) ;
#1447 = CARTESIAN_POINT ( 'NONE',  ( 0.3142011359265306503, -13.17934269988455576, -3.879426116491829557 ) ) ;
#1448 = VERTEX_POINT ( 'NONE', #12732 ) ;
#1449 = CARTESIAN_POINT ( 'NONE',  ( 0.3095370825347234511, -4.681152801286254217, 12.91933430393606486 ) ) ;
#1450 = CARTESIAN_POINT ( 'NONE',  ( 2.048748540252052663, -6.701137625570377843, -11.99999999225501668 ) ) ;
#1451 = EDGE_LOOP ( 'NONE', ( #10350, #9045, #13529, #7763 ) ) ;
#1452 = DIRECTION ( 'NONE',  ( 0.000000000000000000, 0.000000000000000000, -1.000000000000000000 ) ) ;
#1453 = B_SPLINE_CURVE_WITH_KNOTS ( 'NONE', 3,
 ( #2355, #4689, #10976, #12048 ),
 .UNSPECIFIED., .F., .F.,
 ( 4, 4 ),
 ( 0.000000000000000000, 0.002004993803842541195 ),
 .UNSPECIFIED. ) ;
#1454 = DIRECTION ( 'NONE',  ( -0.000000000000000000, -0.000000000000000000, -1.000000000000000000 ) ) ;
#1455 = EDGE_CURVE ( 'NONE', #6145, #14563, #18139, .T. ) ;
#1456 = CARTESIAN_POINT ( 'NONE',  ( 0.3150686449036046444, -4.099563462784746370, 13.11344473514187037 ) ) ;
#1457 = FACE_OUTER_BOUND ( 'NONE', #2813, .T. ) ;
#1458 = EDGE_CURVE ( 'NONE', #4902, #9063, #4904, .T. ) ;
#1459 = EDGE_CURVE ( 'NONE', #1703, #10630, #14916, .T. ) ;
#1460 = CIRCLE ( 'NONE', #12158, 5.000000000000000000 ) ;
#1461 = CARTESIAN_POINT ( 'NONE',  ( 2.369999999999999662, 0.000000000000000000, 0.000000000000000000 ) ) ;
#1462 = CARTESIAN_POINT ( 'NONE',  ( -7.000000000000000000, 8.572527594031473190E-16, 0.000000000000000000 ) ) ;
#1463 = CARTESIAN_POINT ( 'NONE',  ( 0.3058872367615230181, -0.6080468242579999405, -13.72992299905060776 ) ) ;
#1464 = PLANE ( 'NONE',  #11429 ) ;
#1465 = CARTESIAN_POINT ( 'NONE',  ( -66.35602477868047799, 9.999999999999973355, -2.000000000000000000 ) ) ;
#1466 = ORIENTED_EDGE ( 'NONE', *, *, #7516, .T. ) ;
#1467 = CARTESIAN_POINT ( 'NONE',  ( 16.56822296793089322, 0.008619100080558677116, -0.005339139727952955418 ) ) ;
#1468 = ORIENTED_EDGE ( 'NONE', *, *, #9424, .T. ) ;
#1469 = EDGE_LOOP ( 'NONE', ( #658, #13216, #16191 ) ) ;
#1470 = CARTESIAN_POINT ( 'NONE',  ( 1.977436885025663837, -15.04044112860237625, 3.321781585408698056 ) ) ;
#1471 = PRODUCT_DEFINITION ( 'UNKNOWN', '', #4710, #455 ) ;
#1472 = VERTEX_POINT ( 'NONE', #12628 ) ;
#1473 = CARTESIAN_POINT ( 'NONE',  ( 1.861706995891668326, -3.332865258614060355, 12.00328602385079257 ) ) ;
#1474 = EDGE_CURVE ( 'NONE', #11944, #7533, #979, .T. ) ;
#1475 = ORIENTED_EDGE ( 'NONE', *, *, #9024, .T. ) ;
#1476 = CARTESIAN_POINT ( 'NONE',  ( 16.56872352241294521, -0.007240717549633937135, 0.007512283835805527027 ) ) ;
#1477 = B_SPLINE_CURVE_WITH_KNOTS ( 'NONE', 3,
 ( #5144, #8207, #13751, #6587 ),
 .UNSPECIFIED., .F., .F.,
 ( 4, 4 ),
 ( 0.000000000000000000, 0.002004993803842287058 ),
 .UNSPECIFIED. ) ;
#1478 = ADVANCED_FACE ( 'NONE', ( #18646 ), #18461, .F. ) ;
#1479 = EDGE_CURVE ( 'NONE', #15020, #256, #1980, .T. ) ;
#1480 = LINE ( 'NONE', #5326, #547 ) ;
#1481 = B_SPLINE_CURVE_WITH_KNOTS ( 'NONE', 3,
 ( #11747, #17682, #6200, #17871, #10314, #16240 ),
 .UNSPECIFIED., .F., .F.,
 ( 4, 2, 4 ),
 ( 0.000000000000000000, 0.001656992708823241348, 0.003313985417646482697 ),
 .UNSPECIFIED. ) ;
#1482 = CARTESIAN_POINT ( 'NONE',  ( 1.254009781011254265, 9.426200207651111995, 11.25324419414182664 ) ) ;
#1483 = CARTESIAN_POINT ( 'NONE',  ( 1.342453679581834924, -7.902645620902353230, -12.51077660954474702 ) ) ;
#1484 = CARTESIAN_POINT ( 'NONE',  ( 0.3151928476913556376, -8.075547435847033384, 11.11539186930584044 ) ) ;
#1485 = CARTESIAN_POINT ( 'NONE',  ( -194.9999999999999716, 14.99999999999997513, 6.000000000000005329 ) ) ;
#1486 =( BOUNDED_SURFACE ( )  B_SPLINE_SURFACE ( 3, 1, ( 
 ( #16038, #8964 ),
 ( #18706, #1320 ),
 ( #5899, #17279 ),
 ( #2829, #8871 ) ),
 .UNSPECIFIED., .F., .F., .T. ) 
 B_SPLINE_SURFACE_WITH_KNOTS ( ( 4, 4 ),
 ( 2, 2 ),
 ( 0.000000000000000000, 1.000000000000000000 ),
 ( 0.000000000000000000, 1.000000000000000000 ),
 .UNSPECIFIED. ) 
 GEOMETRIC_REPRESENTATION_ITEM ( )  RATIONAL_B_SPLINE_SURFACE ( (
 ( 1.000000000000000000, 1.000000000000000000),
 ( 0.7792777138730160313, 0.9689936506012927220),
 ( 0.7792777138730160313, 0.9689936506012927220),
 ( 1.000000000000000000, 1.000000000000000000) ) ) 
 REPRESENTATION_ITEM ( '' )  SURFACE ( )  );
#1487 =( LENGTH_UNIT ( ) NAMED_UNIT ( * ) SI_UNIT ( .MILLI., .METRE. ) );
#1488 = CARTESIAN_POINT ( 'NONE',  ( 16.58200780006414732, -0.01115192838421568723, -0.0006320991582349211584 ) ) ;
#1489 = CARTESIAN_POINT ( 'NONE',  ( 2.705023505549863483, -3.294610156755986452, 12.88681800078731321 ) ) ;
#1490 = FACE_OUTER_BOUND ( 'NONE', #13629, .T. ) ;
#1491 = CARTESIAN_POINT ( 'NONE',  ( 2.636624412716045196, 11.10302021257998994, -11.60464335004042447 ) ) ;
#1492 = ADVANCED_FACE ( 'NONE', ( #800 ), #9116, .F. ) ;
#1493 = ORIENTED_EDGE ( 'NONE', *, *, #17018, .T. ) ;
#1494 = CARTESIAN_POINT ( 'NONE',  ( 0.4754618798421171855, -8.775436892861030458, -10.80499583390522744 ) ) ;
#1495 = ORIENTED_EDGE ( 'NONE', *, *, #11782, .T. ) ;
#1496 = ORIENTED_EDGE ( 'NONE', *, *, #18440, .T. ) ;
#1497 = ORIENTED_EDGE ( 'NONE', *, *, #5425, .T. ) ;
#1498 = ORIENTED_EDGE ( 'NONE', *, *, #9213, .F. ) ;
#1499 = DIRECTION ( 'NONE',  ( 0.000000000000000000, 0.000000000000000000, 1.000000000000000000 ) ) ;
#1500 = CARTESIAN_POINT ( 'NONE',  ( 16.56679352167444819, -0.009170718284672554205, 0.001518074900131824228 ) ) ;
#1501 = DIRECTION ( 'NONE',  ( 0.000000000000000000, 0.000000000000000000, 1.000000000000000000 ) ) ;
#1502 = ORIENTED_EDGE ( 'NONE', *, *, #17596, .F. ) ;
#1503 = CARTESIAN_POINT ( 'NONE',  ( 0.000000000000000000, -15.99999999999999645, 7.000000000000000000 ) ) ;
#1504 = CARTESIAN_POINT ( 'NONE',  ( 3.512766787570837490, 10.40533104696128497, 10.87507422923887646 ) ) ;
#1505 = FACE_OUTER_BOUND ( 'NONE', #12424, .T. ) ;
#1506 = CARTESIAN_POINT ( 'NONE',  ( 2.747332970342022840, -2.705255688517733681, -16.12459247543629104 ) ) ;
#1507 = CARTESIAN_POINT ( 'NONE',  ( 2.320521194582820801, -15.43440938317095146, -3.126729093671786863 ) ) ;
#1508 = VECTOR ( 'NONE', #17994, 1000.000000000000000 ) ;
#1509 = CIRCLE ( 'NONE', #2412, 14.54644660717763927 ) ;
#1510 = LINE ( 'NONE', #14591, #1685 ) ;
#1511 = FACE_OUTER_BOUND ( 'NONE', #2606, .T. ) ;
#1512 = DIRECTION ( 'NONE',  ( 0.000000000000000000, 0.000000000000000000, -1.000000000000000000 ) ) ;
#1513 = DIRECTION ( 'NONE',  ( 0.000000000000000000, 0.000000000000000000, -1.000000000000000000 ) ) ;
#1514 = AXIS2_PLACEMENT_3D ( 'NONE', #8574, #14398, #8664 ) ;
#1515 = EDGE_CURVE ( 'NONE', #7837, #3148, #11224, .T. ) ;
#1516 = ORIENTED_EDGE ( 'NONE', *, *, #12264, .T. ) ;
#1517 = ORIENTED_EDGE ( 'NONE', *, *, #11103, .F. ) ;
#1518 = VERTEX_POINT ( 'NONE', #13981 ) ;
#1519 = ORIENTED_EDGE ( 'NONE', *, *, #5489, .T. ) ;
#1520 = CARTESIAN_POINT ( 'NONE',  ( 3.950837973638668288, 0.000000000000000000, 0.000000000000000000 ) ) ;
#1521 = ORIENTED_EDGE ( 'NONE', *, *, #16735, .T. ) ;
#1522 = LINE ( 'NONE', #14234, #10985 ) ;
#1523 = CARTESIAN_POINT ( 'NONE',  ( 0.000000000000000000, 0.000000000000000000, 4.750000000000000000 ) ) ;
#1524 = CARTESIAN_POINT ( 'NONE',  ( 0.3095370825347233956, 7.700448427572036181, -11.38092634279620263 ) ) ;
#1525 = CARTESIAN_POINT ( 'NONE',  ( 0.4754618798421167414, 11.68486377711977298, -7.564402563418342496 ) ) ;
#1526 = ORIENTED_EDGE ( 'NONE', *, *, #4878, .F. ) ;
#1527 = CARTESIAN_POINT ( 'NONE',  ( 1.959212340397961327, 0.6675998551413537818, -12.53706137681889388 ) ) ;
#1528 = CARTESIAN_POINT ( 'NONE',  ( 1.845756295923363322, -10.33914852636099191, -6.920504327368305120 ) ) ;
#1529 = DIRECTION ( 'NONE',  ( -0.000000000000000000, 1.000000000000000000, -0.000000000000000000 ) ) ;
#1530 = CARTESIAN_POINT ( 'NONE',  ( 0.4385251269669940277, 8.732456510146231921, -10.76637725024242442 ) ) ;
#1531 = CARTESIAN_POINT ( 'NONE',  ( 0.4862570985993252548, 11.67702470553365401, 7.559321496869467971 ) ) ;
#1532 = EDGE_CURVE ( 'NONE', #10202, #5002, #13321, .T. ) ;
#1533 = CARTESIAN_POINT ( 'NONE',  ( 8.438534575730034959, -5.415535776177550886, 4.221456476902647914 ) ) ;
#1534 = EDGE_CURVE ( 'NONE', #18142, #17352, #5581, .T. ) ;
#1535 = ADVANCED_FACE ( 'NONE', ( #10046 ), #18158, .F. ) ;
#1536 = ORIENTED_EDGE ( 'NONE', *, *, #18056, .T. ) ;
#1537 = CARTESIAN_POINT ( 'NONE',  ( 3.950837973638675393, -10.51028938476224894, 10.05648675950122595 ) ) ;
#1539 = ORIENTED_EDGE ( 'NONE', *, *, #1778, .F. ) ;
#1538 = LINE ( 'NONE', #7377, #13330 ) ;
#1540 = FACE_OUTER_BOUND ( 'NONE', #10498, .T. ) ;
#1541 = ORIENTED_EDGE ( 'NONE', *, *, #7948, .F. ) ;
#1542 = CARTESIAN_POINT ( 'NONE',  ( 3.512766787570702487, -10.87507422923887113, -10.40533104696150701 ) ) ;
#1543 = CARTESIAN_POINT ( 'NONE',  ( 0.7622588538374807099, -7.500000000000000888, -14.39637362139749932 ) ) ;
#1544 = EDGE_CURVE ( 'NONE', #14463, #9042, #14538, .T. ) ;
#1545 = ORIENTED_EDGE ( 'NONE', *, *, #3989, .T. ) ;
#1546 = DIRECTION ( 'NONE',  ( -0.000000000000000000, -0.000000000000000000, 1.000000000000000000 ) ) ;
#1547 = CARTESIAN_POINT ( 'NONE',  ( 3.512766787570759330, -7.127386085302901186, 13.25664064834469968 ) ) ;
#1548 = CARTESIAN_POINT ( 'NONE',  ( 0.3095370825347224519, 10.84046130709058886, 8.444334731364044444 ) ) ;
#1549 = DIRECTION ( 'NONE',  ( 0.000000000000000000, 0.000000000000000000, 1.000000000000000000 ) ) ;
#1550 = B_SPLINE_CURVE_WITH_KNOTS ( 'NONE', 3,
 ( #17558, #9805, #15635, #2537, #8388, #1115 ),
 .UNSPECIFIED., .F., .F.,
 ( 4, 2, 4 ),
 ( 8.673617379884035472E-19, 0.0001828790815886942919, 0.0003657581631773877164 ),
 .UNSPECIFIED. ) ;
#1551 = SURFACE_SIDE_STYLE ('',( #10249 ) ) ;
#1552 = LINE ( 'NONE', #13303, #15949 ) ;
#1553 = CARTESIAN_POINT ( 'NONE',  ( 0.4862570985993235340, 10.79774104611385965, -8.769551628660616771 ) ) ;
#1554 = DIRECTION ( 'NONE',  ( 0.000000000000000000, 0.000000000000000000, 1.000000000000000000 ) ) ;
#1555 = LINE ( 'NONE', #16380, #4099 ) ;
#1556 = PLANE ( 'NONE',  #544 ) ;
#1557 = ADVANCED_FACE ( 'NONE', ( #13197 ), #5201, .F. ) ;
#1558 = ORIENTED_EDGE ( 'NONE', *, *, #2425, .T. ) ;
#1559 = CARTESIAN_POINT ( 'NONE',  ( 1.846138399168762101, -12.43476674860266940, 0.4167076046095114505 ) ) ;
#1560 = ORIENTED_EDGE ( 'NONE', *, *, #10909, .T. ) ;
#1561 = VERTEX_POINT ( 'NONE', #15 ) ;
#1563 = CARTESIAN_POINT ( 'NONE',  ( -194.9999999999999716, -10.00000000000002665, 6.000000000000000000 ) ) ;
#1562 = AXIS2_PLACEMENT_3D ( 'NONE', #11635, #5692, #17463 ) ;
#1564 = ORIENTED_EDGE ( 'NONE', *, *, #11571, .T. ) ;
#1565 = DIRECTION ( 'NONE',  ( 0.000000000000000000, 0.000000000000000000, -1.000000000000000000 ) ) ;
#1566 = VERTEX_POINT ( 'NONE', #9951 ) ;
#1567 = ADVANCED_FACE ( 'NONE', ( #15784 ), #7481, .T. ) ;
#1568 = CARTESIAN_POINT ( 'NONE',  ( 2.636624412714237309, 11.10302021257826866, 11.60464335004050973 ) ) ;
#1569 = CARTESIAN_POINT ( 'NONE',  ( 1.847461586945730261, -7.286856109515127855, 10.08650590720933771 ) ) ;
#1570 = CARTESIAN_POINT ( 'NONE',  ( 16.58200780006414732, -0.007066318000004643239, -0.008650561019685603162 ) ) ;
#1571 = DIRECTION ( 'NONE',  ( 0.7561779333270775005, 0.5081796452863215352, 0.4122479608995760492 ) ) ;
#1572 = B_SPLINE_CURVE_WITH_KNOTS ( 'NONE', 3,
 ( #9403, #1760, #9020, #422 ),
 .UNSPECIFIED., .F., .F.,
 ( 4, 4 ),
 ( 1.117853977359352840E-16, 0.002004993803842554205 ),
 .UNSPECIFIED. ) ;
#1573 = UNCERTAINTY_MEASURE_WITH_UNIT (LENGTH_MEASURE( 1.000000000000000082E-05 ), #18630, 'distance_accuracy_value', 'NONE');
#1574 = CARTESIAN_POINT ( 'NONE',  ( 0.3151930723728413875, -8.137566970826446422, 11.07033375389128871 ) ) ;
#1575 = CARTESIAN_POINT ( 'NONE',  ( 2.636624412714292376, 11.60464335004048309, 11.10302021257707850 ) ) ;
#1576 =( LENGTH_UNIT ( ) NAMED_UNIT ( * ) SI_UNIT ( .MILLI., .METRE. ) );
#1577 = CARTESIAN_POINT ( 'NONE',  ( 1.977436885025821267, -1.488549889121935976, 15.33079650480412326 ) ) ;
#1578 = LINE ( 'NONE', #7419, #10628 ) ;
#1579 = CARTESIAN_POINT ( 'NONE',  ( 0.3170788640506441158, -11.02668139258447866, 8.200855617524497987 ) ) ;
#1580 = CARTESIAN_POINT ( 'NONE',  ( 0.3720661004400040439, 0.7231997263364806638, 13.79610186261030158 ) ) ;
#1581 = CIRCLE ( 'NONE', #1277, 16.06066017081991149 ) ;
#1582 = EDGE_LOOP ( 'NONE', ( #7819, #4815, #18205 ) ) ;
#1583 = VERTEX_POINT ( 'NONE', #11396 ) ;
#1584 = ORIENTED_EDGE ( 'NONE', *, *, #7389, .T. ) ;
#1585 = ORIENTED_EDGE ( 'NONE', *, *, #13107, .F. ) ;
#1586 = EDGE_CURVE ( 'NONE', #1391, #14370, #11676, .T. ) ;
#1587 = FACE_OUTER_BOUND ( 'NONE', #14766, .T. ) ;
#1588 = CARTESIAN_POINT ( 'NONE',  ( 8.438534575730034959, 2.341351102130277528, 6.454982381540297354 ) ) ;
#1589 = FACE_OUTER_BOUND ( 'NONE', #1862, .T. ) ;
#1590 = ORIENTED_EDGE ( 'NONE', *, *, #9778, .T. ) ;
#1591 = LINE ( 'NONE', #7435, #8998 ) ;
#1592 = ADVANCED_FACE ( 'NONE', ( #2677 ), #62, .F. ) ;
#1593 = CARTESIAN_POINT ( 'NONE',  ( -205.0000000000000000, 4.999999999999975131, 3.000000000000002665 ) ) ;
#1594 = CARTESIAN_POINT ( 'NONE',  ( 1.977436885026404134, 10.21547824869624321, -11.52792723756320470 ) ) ;
#1595 = CARTESIAN_POINT ( 'NONE',  ( 0.3720661004400037664, 13.34435358167257313, -3.575426119359045529 ) ) ;
#1596 = CARTESIAN_POINT ( 'NONE',  ( 2.636624412714236865, 0.000000000000000000, 0.000000000000000000 ) ) ;
#1597 = CIRCLE ( 'NONE', #7097, 1.500000000000000000 ) ;
#1598 = CARTESIAN_POINT ( 'NONE',  ( 1.847380140988738484, 11.79969976631077699, -3.949801494731646656 ) ) ;
#1599 = DIRECTION ( 'NONE',  ( 0.7071067818211358436, 0.000000000000000000, -0.7071067805519591909 ) ) ;
#1600 = LINE ( 'NONE', #10200, #6143 ) ;
#1601 = CARTESIAN_POINT ( 'NONE',  ( 0.3151928476913555821, -8.075884471919669849, -11.11514699826559571 ) ) ;
#1602 = ORIENTED_EDGE ( 'NONE', *, *, #2547, .F. ) ;
#1603 = VERTEX_POINT ( 'NONE', #7385 ) ;
#1604 = ORIENTED_EDGE ( 'NONE', *, *, #13965, .F. ) ;
#1605 = EDGE_LOOP ( 'NONE', ( #14578, #7944, #5603, #3741, #6106 ) ) ;
#1606 = CARTESIAN_POINT ( 'NONE',  ( 0.3720661004400040439, -3.575426119359279564, 13.34435358167251984 ) ) ;
#1607 = EDGE_CURVE ( 'NONE', #15230, #1814, #11495, .T. ) ;
#1608 = ORIENTED_EDGE ( 'NONE', *, *, #6091, .F. ) ;
#1609 = LINE ( 'NONE', #7746, #1358 ) ;
#1610 = CARTESIAN_POINT ( 'NONE',  ( 1.847247051441591070, 11.78111530882023317, 4.004229874809065670 ) ) ;
#1611 = FACE_OUTER_BOUND ( 'NONE', #16509, .T. ) ;
#1612 = B_SPLINE_CURVE_WITH_KNOTS ( 'NONE', 3,
 ( #18819, #5715, #1434, #14421, #7173, #10126, #15951, #13085, #8412, #14243, #17199, #8690, #7273 ),
 .UNSPECIFIED., .F., .F.,
 ( 4, 3, 3, 3, 4 ),
 ( 3.144186300207962859E-18, 0.0002299780670421060105, 0.0004599561239687904998, 0.0006896788984287882803, 0.0009194956271626397379 ),
 .UNSPECIFIED. ) ;
#1613 = CARTESIAN_POINT ( 'NONE',  ( 8.438534575730034959, 0.2320579683291088824, -6.862570336891073097 ) ) ;
#1614 = VERTEX_POINT ( 'NONE', #17312 ) ;
#1615 = CARTESIAN_POINT ( 'NONE',  ( -0.1940040276537092212, 7.499999999999998224, -14.18536928022391663 ) ) ;
#1616 = AXIS2_PLACEMENT_3D ( 'NONE', #11781, #21, #15977 ) ;
#1617 = ADVANCED_FACE ( 'NONE', ( #8525 ), #2063, .F. ) ;
#1618 = CARTESIAN_POINT ( 'NONE',  ( 16.56872352241294521, 0.01033355228142499721, 0.001442253899401261912 ) ) ;
#1619 = CARTESIAN_POINT ( 'NONE',  ( 0.4754618798421171855, -7.564402563418553882, 11.68486377711963797 ) ) ;
#1620 = CARTESIAN_POINT ( 'NONE',  ( 2.320521194584406199, 14.32454473830047270, -6.542541239687196253 ) ) ;
#1621 = DIRECTION ( 'NONE',  ( 1.000000000000000000, 0.000000000000000000, 0.000000000000000000 ) ) ;
#1622 = ORIENTED_EDGE ( 'NONE', *, *, #17410, .T. ) ;
#1623 = CARTESIAN_POINT ( 'NONE',  ( 1.847034903785823357, 7.498375632854758166, -9.929438108952064468 ) ) ;
#1625 = ORIENTED_EDGE ( 'NONE', *, *, #5264, .F. ) ;
#1624 = CARTESIAN_POINT ( 'NONE',  ( 0.3151928479966097374, 1.775918418904422640E-15, 13.73922861026898623 ) ) ;
#1626 = DIRECTION ( 'NONE',  ( -1.000000000000000000, -0.000000000000000000, -0.000000000000000000 ) ) ;
#1627 = CIRCLE ( 'NONE', #10178, 5.000000000000000888 ) ;
#1628 = AXIS2_PLACEMENT_3D ( 'NONE', #15591, #9847, #7292 ) ;
#1629 = B_SPLINE_CURVE_WITH_KNOTS ( 'NONE', 3,
 ( #12405, #4960, #15276, #14990 ),
 .UNSPECIFIED., .F., .F.,
 ( 4, 4 ),
 ( 0.000000000000000000, 0.002004993803842899849 ),
 .UNSPECIFIED. ) ;
#1630 = CARTESIAN_POINT ( 'NONE',  ( 0.3095370825347224519, 8.444334731364161684, -10.84046130709049471 ) ) ;
#1631 = B_SPLINE_CURVE_WITH_KNOTS ( 'NONE', 3,
 ( #4696, #3344, #18074, #16639, #10719, #15008 ),
 .UNSPECIFIED., .F., .F.,
 ( 4, 2, 4 ),
 ( 4.016409351050315258E-17, 0.0002014099069817277545, 0.0004028198139634153394 ),
 .UNSPECIFIED. ) ;
#1632 = ORIENTED_EDGE ( 'NONE', *, *, #246, .T. ) ;
#1633 = LINE ( 'NONE', #205, #6254 ) ;
#1634 = CARTESIAN_POINT ( 'NONE',  ( 4.479409541426081276, -7.500000000000000888, -16.64412940056557488 ) ) ;
#1635 = EDGE_LOOP ( 'NONE', ( #3913, #371, #6936, #6859 ) ) ;
#1636 = CARTESIAN_POINT ( 'NONE',  ( 1.560000000000000053, -1.732050807568877859, -1.752539433813135784E-17 ) ) ;
#1637 = ADVANCED_FACE ( 'NONE', ( #2769 ), #14443, .F. ) ;
#1638 = CARTESIAN_POINT ( 'NONE',  ( 2.636624412714236865, 0.000000000000000000, 0.000000000000000000 ) ) ;
#1639 = DIRECTION ( 'NONE',  ( 0.000000000000000000, -1.000000000000000000, 0.000000000000000000 ) ) ;
#1640 = VECTOR ( 'NONE', #17756, 1000.000000000000000 ) ;
#1641 = COLOUR_RGB ( '', 0.66274510, 0.83137255, 0.94901961) ;
#1642 = ORIENTED_EDGE ( 'NONE', *, *, #9893, .F. ) ;
#1643 = CARTESIAN_POINT ( 'NONE',  ( 0.000000000000000000, 0.000000000000000000, 0.000000000000000000 ) ) ;
#1644 = CARTESIAN_POINT ( 'NONE',  ( 3.950837973638668288, 0.000000000000000000, 0.000000000000000000 ) ) ;
#1645 = CARTESIAN_POINT ( 'NONE',  ( 0.3058872367615230181, -13.24582953854922529, -3.664492643742902178 ) ) ;
#1646 = CARTESIAN_POINT ( 'NONE',  ( 0.000000000000000000, 0.000000000000000000, -3.000000000000000000 ) ) ;
#1647 = CARTESIAN_POINT ( 'NONE',  ( 0.3137051932979792457, 7.698472063774471685, 11.37800749014133928 ) ) ;
#1648 = ORIENTED_EDGE ( 'NONE', *, *, #11206, .F. ) ;
#1649 = CARTESIAN_POINT ( 'NONE',  ( 0.3137051932979809665, -4.679953077377580151, 12.91601973349268917 ) ) ;
#1650 = CARTESIAN_POINT ( 'NONE',  ( 2.636624412715137922, -14.46769361191291559, 6.973567714907789927 ) ) ;
#1651 = VERTEX_POINT ( 'NONE', #10339 ) ;
#1652 = VERTEX_POINT ( 'NONE', #13006 ) ;
#1653 = CARTESIAN_POINT ( 'NONE',  ( 0.4384471787762845851, -4.978024343488958614, -12.93784327393178302 ) ) ;
#1654 = VECTOR ( 'NONE', #17324, 1000.000000000000000 ) ;
#1655 = ORIENTED_EDGE ( 'NONE', *, *, #1264, .T. ) ;
#1656 = CARTESIAN_POINT ( 'NONE',  ( 1.846138399168762989, -3.446241763653083101, 11.95493567637849530 ) ) ;
#1657 = VERTEX_POINT ( 'NONE', #4321 ) ;
#1658 = EDGE_CURVE ( 'NONE', #3963, #18321, #8990, .T. ) ;
#1659 = EDGE_CURVE ( 'NONE', #11688, #11324, #401, .T. ) ;
#1660 = ADVANCED_FACE ( 'NONE', ( #11871 ), #4607, .F. ) ;
#1661 = CARTESIAN_POINT ( 'NONE',  ( 1.861706995891668992, -11.66987142852987169, 4.359009869687201721 ) ) ;
#1662 = FACE_OUTER_BOUND ( 'NONE', #1442, .T. ) ;
#1663 = CARTESIAN_POINT ( 'NONE',  ( 0.4754618798421171855, 3.583352865732860604, -13.45049478164055756 ) ) ;
#1664 = CARTESIAN_POINT ( 'NONE',  ( 1.959212340397946006, -4.509090217468600947, 11.71715421693496673 ) ) ;
#1665 = B_SPLINE_CURVE_WITH_KNOTS ( 'NONE', 3,
 ( #4489, #16144, #10406, #1325, #17576, #14800 ),
 .UNSPECIFIED., .F., .F.,
 ( 4, 2, 4 ),
 ( 0.000000000000000000, 0.001656992708822777310, 0.003313985417645554619 ),
 .UNSPECIFIED. ) ;
#1666 = CARTESIAN_POINT ( 'NONE',  ( 2.636624412715999011, 2.161493821598055920, -15.91454522070273647 ) ) ;
#1667 = CARTESIAN_POINT ( 'NONE',  ( 2.320520222538862143, 13.71278186123479870, -7.743191299716691844 ) ) ;
#1668 = AXIS2_PLACEMENT_3D ( 'NONE', #5688, #15832, #14585 ) ;
#1669 = DIRECTION ( 'NONE',  ( 0.000000000000000000, 0.000000000000000000, -1.000000000000000000 ) ) ;
#1670 = CARTESIAN_POINT ( 'NONE',  ( 1.560000000000000053, 0.8660254037844389297, 1.500000000000000000 ) ) ;
#1671 = VECTOR ( 'NONE', #15487, 1000.000000000000114 ) ;
#1672 = B_SPLINE_CURVE_WITH_KNOTS ( 'NONE', 3,
 ( #11666, #8607, #4397, #14432 ),
 .UNSPECIFIED., .F., .F.,
 ( 4, 4 ),
 ( 1.182319362138779820E-16, 0.002004993803842621859 ),
 .UNSPECIFIED. ) ;
#1673 = CARTESIAN_POINT ( 'NONE',  ( 0.4754618798421171855, 11.68486377711966639, 7.564402563418515690 ) ) ;
#1674 = CIRCLE ( 'NONE', #2565, 3.499999999999992895 ) ;
#1675 = CARTESIAN_POINT ( 'NONE',  ( 1.342453679581834924, -13.74702459364880269, -5.476372339890162699 ) ) ;
#1676 = CARTESIAN_POINT ( 'NONE',  ( 1.847461586945728929, -11.82388984758122064, 3.877048136045332605 ) ) ;
#1677 = CARTESIAN_POINT ( 'NONE',  ( 16.56782317627811096, -0.005492611183758475124, -0.008141063682853461742 ) ) ;
#1678 = B_SPLINE_CURVE_WITH_KNOTS ( 'NONE', 3,
 ( #8570, #7053, #8767, #11540, #9999, #13058 ),
 .UNSPECIFIED., .F., .F.,
 ( 4, 2, 4 ),
 ( 7.047314121155778821E-19, 0.001657017934710171237, 0.003314035869420342041 ),
 .UNSPECIFIED. ) ;
#1679 = ORIENTED_EDGE ( 'NONE', *, *, #4558, .F. ) ;
#1680 = ORIENTED_EDGE ( 'NONE', *, *, #12410, .F. ) ;
#1681 = EDGE_LOOP ( 'NONE', ( #2116, #2959, #6082, #2082 ) ) ;
#1682 = ORIENTED_EDGE ( 'NONE', *, *, #4053, .F. ) ;
#1683 = DIRECTION ( 'NONE',  ( 0.000000000000000000, 0.000000000000000000, 1.000000000000000000 ) ) ;
#1684 = AXIS2_PLACEMENT_3D ( 'NONE', #9479, #10822, #6338 ) ;
#1685 = VECTOR ( 'NONE', #6293, 1000.000000000000000 ) ;
#1686 = B_SPLINE_CURVE_WITH_KNOTS ( 'NONE', 3,
 ( #11949, #16251, #3132, #17784, #17880, #9082 ),
 .UNSPECIFIED., .F., .F.,
 ( 4, 2, 4 ),
 ( 0.000000000000000000, 0.001656992708821696143, 0.003313985417643392287 ),
 .UNSPECIFIED. ) ;
#1687 = CARTESIAN_POINT ( 'NONE',  ( 1.846613052777651198, -12.43780859207240042, 0.3401093050881381363 ) ) ;
#1688 = EDGE_LOOP ( 'NONE', ( #13705, #9023, #13242, #14848 ) ) ;
#1689 = DIRECTION ( 'NONE',  ( -0.000000000000000000, -1.000000000000000000, -0.000000000000000000 ) ) ;
#1690 = CARTESIAN_POINT ( 'NONE',  ( -30.00000000000000355, -12.50000000000000178, -7.071067811865460406 ) ) ;
#1691 = ADVANCED_FACE ( 'NONE', ( #505 ), #5914, .F. ) ;
#1692 = CARTESIAN_POINT ( 'NONE',  ( 16.56753206892534891, 0.004368917149005337522, 0.008432171035096464387 ) ) ;
#1693 = CARTESIAN_POINT ( 'NONE',  ( 3.950837973638677170, -1.958075594453692503, -14.41405733518062959 ) ) ;
#1694 = CARTESIAN_POINT ( 'NONE',  ( 1.846138399168762101, 12.43476674860266584, -0.4167076046095982700 ) ) ;
#1695 = CARTESIAN_POINT ( 'NONE',  ( 1.846955891736114852, 11.74973605926570386, -4.094751675596581819 ) ) ;
#1696 = CARTESIAN_POINT ( 'NONE',  ( 2.320520222537280741, -6.542539914240626864, 14.32454429810376162 ) ) ;
#1697 = CARTESIAN_POINT ( 'NONE',  ( 0.3308579732647026761, -12.88563776947742312, -4.812490080619330257 ) ) ;
#1698 = CARTESIAN_POINT ( 'NONE',  ( 25.00000000000000000, -2.500000000000000444, -17.00000000000000000 ) ) ;
#1699 = ORIENTED_EDGE ( 'NONE', *, *, #9940, .T. ) ;
#1700 = VECTOR ( 'NONE', #15659, 1000.000000000000000 ) ;
#1701 = AXIS2_PLACEMENT_3D ( 'NONE', #9909, #18518, #5427 ) ;
#1702 = ORIENTED_EDGE ( 'NONE', *, *, #5723, .T. ) ;
#1703 = VERTEX_POINT ( 'NONE', #3351 ) ;
#1704 = ORIENTED_EDGE ( 'NONE', *, *, #3086, .F. ) ;
#1705 = CARTESIAN_POINT ( 'NONE',  ( 0.3095370825347234511, 13.73357284481724783, 0.4597470195090685441 ) ) ;
#1706 = ORIENTED_EDGE ( 'NONE', *, *, #17242, .F. ) ;
#1707 = CARTESIAN_POINT ( 'NONE',  ( 0.3137051932979757485, -11.37800749014125223, -7.698472063774596030 ) ) ;
#1708 = DIRECTION ( 'NONE',  ( 0.000000000000000000, -1.000000000000000000, 0.000000000000000000 ) ) ;
#1709 = CARTESIAN_POINT ( 'NONE',  ( 2.747332970342022840, 14.63517873738947195, 7.289199830147158998 ) ) ;
#1710 = EDGE_CURVE ( 'NONE', #9189, #11716, #4983, .T. ) ;
#1711 = CARTESIAN_POINT ( 'NONE',  ( 2.002547531651519996, 0.6781519942173496185, -12.57989064830758785 ) ) ;
#1712 = VERTEX_POINT ( 'NONE', #3449 ) ;
#1713 = CARTESIAN_POINT ( 'NONE',  ( 0.3137051932979792457, -0.4596302728640728752, 13.73004976592201842 ) ) ;
#1714 = FACE_OUTER_BOUND ( 'NONE', #11824, .T. ) ;
#1715 = EDGE_CURVE ( 'NONE', #13002, #14390, #9283, .T. ) ;
#1716 = CIRCLE ( 'NONE', #6298, 5.000000000000000888 ) ;
#1717 = PLANE ( 'NONE',  #10053 ) ;
#1718 = CARTESIAN_POINT ( 'NONE',  ( 1.847247051441591514, -10.16425585218606109, 7.177495230324669961 ) ) ;
#1719 =( GEOMETRIC_REPRESENTATION_CONTEXT ( 3 ) GLOBAL_UNCERTAINTY_ASSIGNED_CONTEXT ( ( #13193 ) ) GLOBAL_UNIT_ASSIGNED_CONTEXT ( ( #14378, #12665, #4064 ) ) REPRESENTATION_CONTEXT ( 'NONE', 'WORKASPACE' ) );
#1720 = B_SPLINE_CURVE_WITH_KNOTS ( 'NONE', 3,
 ( #9046, #10383, #4748, #17652, #16419, #4559, #352, #14875, #6281, #3100 ),
 .UNSPECIFIED., .F., .F.,
 ( 4, 3, 3, 4 ),
 ( 0.0004597478348664300451, 0.0004599561239687907166, 0.0006896788984287883888, 0.0009194956271626400631 ),
 .UNSPECIFIED. ) ;
#1721 = PLANE ( 'NONE',  #4737 ) ;
#1722 = CARTESIAN_POINT ( 'NONE',  ( 0.3145729642390426295, 13.15786090015083687, 3.952965287571154729 ) ) ;
#1723 = CARTESIAN_POINT ( 'NONE',  ( 16.56753206892534891, -0.001549402974393209202, 0.009369540855502124857 ) ) ;
#1724 = ORIENTED_EDGE ( 'NONE', *, *, #586, .F. ) ;
#1725 = CARTESIAN_POINT ( 'NONE',  ( 1.846138399168762101, 7.646096044340033870, -9.815003036200328879 ) ) ;
#1727 = ORIENTED_EDGE ( 'NONE', *, *, #3988, .F. ) ;
#1726 = CARTESIAN_POINT ( 'NONE',  ( 2.705023505549865703, 11.23800170568056878, 7.115606223895208693 ) ) ;
#1728 = CARTESIAN_POINT ( 'NONE',  ( 1.959283090834841090, 11.71721539537261414, -4.509128209890848282 ) ) ;
#1729 = EDGE_CURVE ( 'NONE', #10438, #8651, #15823, .T. ) ;
#1730 = AXIS2_PLACEMENT_3D ( 'NONE', #2023, #7862, #7960 ) ;
#1731 = CARTESIAN_POINT ( 'NONE',  ( 16.56822296793089322, -0.002414375228568327748, 0.009847136207496262617 ) ) ;
#1732 = CIRCLE ( 'NONE', #14545, 0.5000000000000004441 ) ;
#1733 = EDGE_LOOP ( 'NONE', ( #13246, #1019, #8676, #6333 ) ) ;
#1734 = ADVANCED_FACE ( 'NONE', ( #15115 ), #6555, .F. ) ;
#1735 = DIRECTION ( 'NONE',  ( -0.8629742774544859607, 0.5052478564545405115, 0.000000000000000000 ) ) ;
#1736 = UNCERTAINTY_MEASURE_WITH_UNIT (LENGTH_MEASURE( 1.000000000000000082E-05 ), #1576, 'distance_accuracy_value', 'NONE');
#1737 = CARTESIAN_POINT ( 'NONE',  ( 6.265543861956754057, -7.499999999999872990, -12.41474642440651621 ) ) ;
#1738 = ORIENTED_EDGE ( 'NONE', *, *, #18088, .F. ) ;
#1739 = CARTESIAN_POINT ( 'NONE',  ( 2.705023505549866591, -11.23800170568051371, -7.115606223895292182 ) ) ;
#1740 = CARTESIAN_POINT ( 'NONE',  ( 3.950837973638677170, 1.958075594453790869, 14.41405733518061538 ) ) ;
#1741 = VECTOR ( 'NONE', #13870, 1000.000000000000000 ) ;
#1742 = CARTESIAN_POINT ( 'NONE',  ( 0.4862570985993235340, -8.769551628660655851, -10.79774104611382946 ) ) ;
#1743 = DIRECTION ( 'NONE',  ( 1.000000000000000000, 0.000000000000000000, 0.000000000000000000 ) ) ;
#1744 = CIRCLE ( 'NONE', #12429, 2.375000000000000444 ) ;
#1745 = AXIS2_PLACEMENT_3D ( 'NONE', #8090, #7914, #16505 ) ;
#1746 = VERTEX_POINT ( 'NONE', #12253 ) ;
#1747 = CLOSED_SHELL ( 'NONE', ( #3095, #17796, #12636, #7500, #4544, #6621, #1213, #10594, #18722, #17795, #18340, #215, #6090, #6941 ) ) ;
#1748 = EDGE_CURVE ( 'NONE', #3711, #4894, #334, .T. ) ;
#1749 = CARTESIAN_POINT ( 'NONE',  ( 1.846138399168762101, -10.30487220521574976, 6.971848976710974810 ) ) ;
#1750 = CARTESIAN_POINT ( 'NONE',  ( 0.4754618798421162973, -0.7484603771383456783, -13.89949764182683545 ) ) ;
#1751 = LINE ( 'NONE', #16478, #16323 ) ;
#1752 = DIRECTION ( 'NONE',  ( 0.000000000000000000, 0.000000000000000000, 1.000000000000000000 ) ) ;
#1753 = EDGE_CURVE ( 'NONE', #8074, #12492, #16369, .T. ) ;
#1754 = ORIENTED_EDGE ( 'NONE', *, *, #15943, .T. ) ;
#1755 = CARTESIAN_POINT ( 'NONE',  ( 2.747332970342022840, -7.555624153089749662, 14.49942876448589679 ) ) ;
#1756 = FACE_OUTER_BOUND ( 'NONE', #7700, .T. ) ;
#1757 = ORIENTED_EDGE ( 'NONE', *, *, #9650, .F. ) ;
#1758 = VECTOR ( 'NONE', #10835, 1000.000000000000114 ) ;
#1759 = ORIENTED_EDGE ( 'NONE', *, *, #2129, .F. ) ;
#1760 = CARTESIAN_POINT ( 'NONE',  ( 3.074695600507308946, 2.093687500611960850, 15.41438262616221522 ) ) ;
#1761 = ORIENTED_EDGE ( 'NONE', *, *, #7020, .T. ) ;
#1762 = CARTESIAN_POINT ( 'NONE',  ( 1.918918678667047129, -3.258447776119917094, 12.08296592096907318 ) ) ;
#1763 = ORIENTED_EDGE ( 'NONE', *, *, #10294, .T. ) ;
#1764 = FILL_AREA_STYLE ('',( #3572 ) ) ;
#1765 =( LENGTH_UNIT ( ) NAMED_UNIT ( * ) SI_UNIT ( .MILLI., .METRE. ) );
#1766 = CARTESIAN_POINT ( 'NONE',  ( 16.56753206892534891, -0.004368917149005391298, -0.008432171035096433162 ) ) ;
#1767 =( BOUNDED_SURFACE ( )  B_SPLINE_SURFACE ( 3, 1, ( 
 ( #15221, #2134 ),
 ( #13780, #6800 ),
 ( #12617, #1152 ),
 ( #15667, #15304 ) ),
 .UNSPECIFIED., .F., .F., .T. ) 
 B_SPLINE_SURFACE_WITH_KNOTS ( ( 4, 4 ),
 ( 2, 2 ),
 ( 0.000000000000000000, 1.000000000000000000 ),
 ( 0.000000000000000000, 1.000000000000000000 ),
 .UNSPECIFIED. ) 
 GEOMETRIC_REPRESENTATION_ITEM ( )  RATIONAL_B_SPLINE_SURFACE ( (
 ( 1.000000000000000000, 1.000000000000000000),
 ( 0.7792777138730158093, 0.9689936506012928330),
 ( 0.7792777138730158093, 0.9689936506012928330),
 ( 1.000000000000000000, 1.000000000000000000) ) ) 
 REPRESENTATION_ITEM ( '' )  SURFACE ( )  );
#1768 = CARTESIAN_POINT ( 'NONE',  ( 2.320521194584054037, 7.743190876765937425, -13.71278319228217946 ) ) ;
#1769 = CIRCLE ( 'NONE', #1145, 14.54644660717763927 ) ;
#1770 = DIRECTION ( 'NONE',  ( 0.7635533937278214944, -0.3966532189476670300, 0.5095610256143814354 ) ) ;
#1771 = PLANE ( 'NONE',  #5356 ) ;
#1772 =( NAMED_UNIT ( * ) PLANE_ANGLE_UNIT ( ) SI_UNIT ( $, .RADIAN. ) );
#1773 = CARTESIAN_POINT ( 'NONE',  ( 0.000000000000000000, 0.000000000000000000, 0.000000000000000000 ) ) ;
#1774 = DIRECTION ( 'NONE',  ( -0.000000000000000000, -0.000000000000000000, 1.000000000000000000 ) ) ;
#1775 = CARTESIAN_POINT ( 'NONE',  ( 2.123976203522053741, 6.261444813538558307, 14.31368049382972529 ) ) ;
#1776 = CARTESIAN_POINT ( 'NONE',  ( 3.950837973638676281, 10.05648675950141602, -10.51028938476206953 ) ) ;
#1777 = EDGE_CURVE ( 'NONE', #13145, #12510, #1840, .T. ) ;
#1778 = EDGE_CURVE ( 'NONE', #1652, #6835, #5758, .T. ) ;
#1779 = EDGE_CURVE ( 'NONE', #2783, #5819, #16527, .T. ) ;
#1780 = CARTESIAN_POINT ( 'NONE',  ( 0.3095370825347224519, 12.91933430393614302, -4.681152801286025955 ) ) ;
#1781 = CARTESIAN_POINT ( 'NONE',  ( 2.002547531651519996, -12.17374746633575988, -3.242439124566779185 ) ) ;
#1782 = ORIENTED_EDGE ( 'NONE', *, *, #7144, .F. ) ;
#1783 = AXIS2_PLACEMENT_3D ( 'NONE', #17178, #14226, #10108 ) ;
#1784 = VERTEX_POINT ( 'NONE', #6794 ) ;
#1785 = ORIENTED_EDGE ( 'NONE', *, *, #12342, .T. ) ;
#1786 = ORIENTED_EDGE ( 'NONE', *, *, #10512, .T. ) ;
#1787 = CARTESIAN_POINT ( 'NONE',  ( 0.000000000000000000, 0.000000000000000000, 10.50000000000000000 ) ) ;
#1788 = PLANE ( 'NONE',  #4428 ) ;
#1789 = CARTESIAN_POINT ( 'NONE',  ( 1.845755665166724846, -3.386720041070645948, -11.97169564665394681 ) ) ;
#1790 = EDGE_CURVE ( 'NONE', #2855, #2106, #2387, .T. ) ;
#1791 = VECTOR ( 'NONE', #975, 1000.000000000000000 ) ;
#1792 = CARTESIAN_POINT ( 'NONE',  ( 0.3132642857406528480, 13.72733058964895037, 0.5276792104582755938 ) ) ;
#1793 = CARTESIAN_POINT ( 'NONE',  ( 0.000000000000000000, 0.000000000000000000, -3.000000000000000000 ) ) ;
#1794 = CARTESIAN_POINT ( 'NONE',  ( 16.56782317627811096, 0.005492611183758417011, 0.008141063682853501640 ) ) ;
#1795 = CARTESIAN_POINT ( 'NONE',  ( -33.99999999999999289, -12.50000000000000178, 6.500000000000000888 ) ) ;
#1796 = CARTESIAN_POINT ( 'NONE',  ( 1.847372867223025628, 12.44269075185938789, 0.1054171785006922379 ) ) ;
#1797 = CARTESIAN_POINT ( 'NONE',  ( 1.845756295923360435, -4.296776483139397307, -11.67600463554277468 ) ) ;
#1798 = CARTESIAN_POINT ( 'NONE',  ( 1.562796894703937678, 0.000000000000000000, -12.15840553252917289 ) ) ;
#1799 = PLANE ( 'NONE',  #7889 ) ;
#1800 =( NAMED_UNIT ( * ) SI_UNIT ( $, .STERADIAN. ) SOLID_ANGLE_UNIT ( ) );
#1801 = CARTESIAN_POINT ( 'NONE',  ( 0.3145729642390391878, -8.321438378985172690, -10.93201268464381748 ) ) ;
#1802 = ORIENTED_EDGE ( 'NONE', *, *, #3840, .F. ) ;
#1803 = ORIENTED_EDGE ( 'NONE', *, *, #4909, .T. ) ;
#1804 = EDGE_CURVE ( 'NONE', #14815, #17303, #10104, .T. ) ;
#1805 = ORIENTED_EDGE ( 'NONE', *, *, #11183, .F. ) ;
#1806 = EDGE_CURVE ( 'NONE', #14209, #13318, #2642, .T. ) ;
#1807 = VERTEX_POINT ( 'NONE', #17106 ) ;
#1808 = CARTESIAN_POINT ( 'NONE',  ( 2.636624412717099908, 14.46769361191384817, -6.973567714910368309 ) ) ;
#1809 = DIRECTION ( 'NONE',  ( 0.000000000000000000, 1.000000000000000000, -0.000000000000000000 ) ) ;
#1810 = CARTESIAN_POINT ( 'NONE',  ( 0.000000000000000000, 0.000000000000000000, 0.000000000000000000 ) ) ;
#1811 = CARTESIAN_POINT ( 'NONE',  ( -194.9999999999999716, -30.00000000000003197, 3.000000000000000000 ) ) ;
#1812 = AXIS2_PLACEMENT_3D ( 'NONE', #15485, #781, #18442 ) ;
#1813 = CARTESIAN_POINT ( 'NONE',  ( -53.40568638168567617, 9.314871387272408043, 6.000000000000000000 ) ) ;
#1814 = VERTEX_POINT ( 'NONE', #4011 ) ;
#1815 = LINE ( 'NONE', #382, #16634 ) ;
#1816 = EDGE_CURVE ( 'NONE', #15520, #5678, #15774, .T. ) ;
#1817 = CARTESIAN_POINT ( 'NONE',  ( 1.560000000000000053, 1.732050807568878747, 7.017607234860990640E-28 ) ) ;
#1818 = DIRECTION ( 'NONE',  ( -0.000000000000000000, -0.000000000000000000, 1.000000000000000000 ) ) ;
#1819 = CARTESIAN_POINT ( 'NONE',  ( 0.4754618798421162973, 12.98792082933644743, 5.007009103465295929 ) ) ;
#1820 = CONICAL_SURFACE ( 'NONE', #7320, 14.54644660717763927, 0.8559913436420816257 ) ;
#1821 = DIRECTION ( 'NONE',  ( -1.000000000000000000, -0.000000000000000000, -0.000000000000000000 ) ) ;
#1822 = CARTESIAN_POINT ( 'NONE',  ( 16.56753206892534891, 0.008490833999798920451, 0.004253784598196212220 ) ) ;
#1823 = EDGE_LOOP ( 'NONE', ( #3640, #8517, #8869, #3051 ) ) ;
#1824 = VECTOR ( 'NONE', #11466, 1000.000000000000000 ) ;
#1825 = EDGE_CURVE ( 'NONE', #16257, #13262, #3510, .T. ) ;
#1826 = DIRECTION ( 'NONE',  ( 0.000000000000000000, -1.224646799147353207E-16, 1.000000000000000000 ) ) ;
#1828 = ORIENTED_EDGE ( 'NONE', *, *, #2662, .T. ) ;
#1827 = CARTESIAN_POINT ( 'NONE',  ( 0.3151928478948580192, 0.0001388664989280257334, 13.73922860964089665 ) ) ;
#1829 = CARTESIAN_POINT ( 'NONE',  ( -25.00000000000000000, 2.499999999999998668, -12.00000000000000000 ) ) ;
#1830 = ORIENTED_EDGE ( 'NONE', *, *, #6341, .T. ) ;
#1831 = EDGE_CURVE ( 'NONE', #16711, #12401, #4496, .T. ) ;
#1832 = EDGE_CURVE ( 'NONE', #16531, #4154, #12338, .T. ) ;
#1833 = B_SPLINE_CURVE_WITH_KNOTS ( 'NONE', 3,
 ( #7807, #12198, #3583, #18023, #15152, #4927 ),
 .UNSPECIFIED., .F., .F.,
 ( 4, 2, 4 ),
 ( 4.269227611140977934E-17, 0.0002014099069817279985, 0.0004028198139634133336 ),
 .UNSPECIFIED. ) ;
#1834 = DIRECTION ( 'NONE',  ( -0.7635533937278214944, -0.6071939193889592801, 0.2197766120036439286 ) ) ;
#1835 = ORIENTED_EDGE ( 'NONE', *, *, #3867, .T. ) ;
#1836 = CARTESIAN_POINT ( 'NONE',  ( 0.4862570985993235340, -13.89016912371018186, 0.7479633556561964269 ) ) ;
#1837 = CARTESIAN_POINT ( 'NONE',  ( 3.431439422793015392, -6.119758975832682246, -11.99999999209394907 ) ) ;
#1838 = EDGE_CURVE ( 'NONE', #9063, #287, #6935, .T. ) ;
#1839 = ORIENTED_EDGE ( 'NONE', *, *, #12750, .F. ) ;
#1840 = LINE ( 'NONE', #7678, #220 ) ;
#1841 = CARTESIAN_POINT ( 'NONE',  ( 0.3151930723728450512, 13.73922999529477451, 0.07645105376991474799 ) ) ;
#1842 = CARTESIAN_POINT ( 'NONE',  ( 16.56753206892534891, -0.009389754735542257466, -0.001421777558675915579 ) ) ;
#1843 = CARTESIAN_POINT ( 'NONE',  ( -6.000000000000000000, 20.00000000000000000, 4.000000000000000000 ) ) ;
#1844 = ADVANCED_FACE ( 'NONE', ( #14055 ), #5167, .T. ) ;
#1845 = SURFACE_STYLE_USAGE ( .BOTH. , #6526 ) ;
#1846 = CARTESIAN_POINT ( 'NONE',  ( 1.342453679581834924, -12.51077660954471504, 7.902645620902405632 ) ) ;
#1847 = CARTESIAN_POINT ( 'NONE',  ( 0.3148213771069381384, 10.97836617636225220, 8.260246460850757089 ) ) ;
#1848 = B_SPLINE_CURVE_WITH_KNOTS ( 'NONE', 3,
 ( #1991, #12481, #16525, #464, #13650, #3411 ),
 .UNSPECIFIED., .F., .F.,
 ( 4, 2, 4 ),
 ( 0.000000000000000000, 0.0001828790815886945087, 0.0003657581631773890174 ),
 .UNSPECIFIED. ) ;
#1849 = CARTESIAN_POINT ( 'NONE',  ( 2.750000000000000000, 0.000000000000000000, 0.000000000000000000 ) ) ;
#1851 = ORIENTED_EDGE ( 'NONE', *, *, #13046, .F. ) ;
#1850 = DIRECTION ( 'NONE',  ( 1.000000000000000000, 0.000000000000000000, 0.000000000000000000 ) ) ;
#1852 = CARTESIAN_POINT ( 'NONE',  ( 1.846138399168762101, -11.69739621335925328, 4.238866729160359448 ) ) ;
#1853 = EDGE_LOOP ( 'NONE', ( #6438, #10768, #2357, #755 ) ) ;
#1854 = CARTESIAN_POINT ( 'NONE',  ( 3.950837973638668288, 0.000000000000000000, 0.000000000000000000 ) ) ;
#1855 = CARTESIAN_POINT ( 'NONE',  ( 0.3170788640506441158, -11.02668139258447866, 8.200855617524497987 ) ) ;
#1856 = ORIENTED_EDGE ( 'NONE', *, *, #10608, .T. ) ;
#1857 = AXIS2_PLACEMENT_3D ( 'NONE', #13320, #13613, #18017 ) ;
#1858 = VERTEX_POINT ( 'NONE', #16742 ) ;
#1859 = DIRECTION ( 'NONE',  ( 0.000000000000000000, 0.000000000000000000, 1.000000000000000000 ) ) ;
#1860 = VERTEX_POINT ( 'NONE', #9746 ) ;
#1861 = CARTESIAN_POINT ( 'NONE',  ( 0.000000000000000000, 0.000000000000000000, 3.000000000000000000 ) ) ;
#1862 = EDGE_LOOP ( 'NONE', ( #3776, #7335, #13877, #5146 ) ) ;
#1863 = EDGE_CURVE ( 'NONE', #16885, #9189, #8144, .T. ) ;
#1864 = DIRECTION ( 'NONE',  ( 0.7635533937278214944, -0.6204116510013502062, 0.1790966170213858510 ) ) ;
#1865 = CARTESIAN_POINT ( 'NONE',  ( 0.3720661004400040439, -13.79610186261030513, 0.7231997263364323691 ) ) ;
#1866 = B_SPLINE_CURVE_WITH_KNOTS ( 'NONE', 3,
 ( #14778, #8858, #1594, #11729, #17559, #7437 ),
 .UNSPECIFIED., .F., .F.,
 ( 4, 2, 4 ),
 ( 0.000000000000000000, 0.001656992708823241348, 0.003313985417646482697 ),
 .UNSPECIFIED. ) ;
#1867 = CARTESIAN_POINT ( 'NONE',  ( 2.636624412715999011, 2.161493821598055920, -15.91454522070273647 ) ) ;
#1868 = DIRECTION ( 'NONE',  ( -1.000000000000000000, -1.387778780781445676E-15, 0.000000000000000000 ) ) ;
#1869 = ADVANCED_FACE ( 'NONE', ( #12519 ), #10124, .F. ) ;
#1870 = PLANE ( 'NONE',  #10860 ) ;
#1871 = CARTESIAN_POINT ( 'NONE',  ( -58.82978549640777288, -10.68512861272757952, 6.000000000000000000 ) ) ;
#1872 = CARTESIAN_POINT ( 'NONE',  ( 2.697797270744667131, 13.26309265156977624, 0.9169917281807724585 ) ) ;
#1873 = LINE ( 'NONE', #10858, #17961 ) ;
#1874 = CARTESIAN_POINT ( 'NONE',  ( 1.847380140988740260, 7.224522571381473135, -10.13114603776188893 ) ) ;
#1875 = CARTESIAN_POINT ( 'NONE',  ( 3.353306896162455697, 12.78841260990237672, 5.573563251762143622 ) ) ;
#1876 = VECTOR ( 'NONE', #4466, 1000.000000000000000 ) ;
#1877 = CARTESIAN_POINT ( 'NONE',  ( 16.56679352167444819, -0.009190982326619374226, 0.001390132774595425865 ) ) ;
#1878 = CARTESIAN_POINT ( 'NONE',  ( 16.56872352241294521, -0.01027347319884365333, -0.001821578298043897851 ) ) ;
#1879 = EDGE_LOOP ( 'NONE', ( #6954, #17432, #9993, #15185 ) ) ;
#1880 = ORIENTED_EDGE ( 'NONE', *, *, #10677, .F. ) ;
#1881 = EDGE_LOOP ( 'NONE', ( #8452, #16560, #5178, #17650, #3158, #7094, #9920, #7769 ) ) ;
#1882 = EDGE_LOOP ( 'NONE', ( #10890, #7353 ) ) ;
#1883 = B_SPLINE_CURVE_WITH_KNOTS ( 'NONE', 3,
 ( #4717, #2041, #15030, #4816 ),
 .UNSPECIFIED., .F., .F.,
 ( 4, 4 ),
 ( 5.210130127421859526E-17, 0.002004993803842660023 ),
 .UNSPECIFIED. ) ;
#1884 =( BOUNDED_SURFACE ( )  B_SPLINE_SURFACE ( 3, 1, ( 
 ( #2159, #7997 ),
 ( #11046, #18206 ),
 ( #10955, #16773 ),
 ( #12466, #18296 ) ),
 .UNSPECIFIED., .F., .F., .T. ) 
 B_SPLINE_SURFACE_WITH_KNOTS ( ( 4, 4 ),
 ( 2, 2 ),
 ( 0.000000000000000000, 1.000000000000000000 ),
 ( 0.000000000000000000, 1.000000000000000000 ),
 .UNSPECIFIED. ) 
 GEOMETRIC_REPRESENTATION_ITEM ( )  RATIONAL_B_SPLINE_SURFACE ( (
 ( 1.000000000000000000, 1.000000000000000000),
 ( 0.9933953342250438912, 0.8357391271907739227),
 ( 0.9933953342250438912, 0.8357391271907739227),
 ( 1.000000000000000000, 1.000000000000000000) ) ) 
 REPRESENTATION_ITEM ( '' )  SURFACE ( )  );
#1885 = CARTESIAN_POINT ( 'NONE',  ( 2.002547531651519996, -12.17374746633580784, 3.242439124566603326 ) ) ;
#1886 = FACE_OUTER_BOUND ( 'NONE', #200, .T. ) ;
#1887 = CARTESIAN_POINT ( 'NONE',  ( 2.353870697619111052, -12.05847592522640355, -4.720869121224258613 ) ) ;
#1888 = DIRECTION ( 'NONE',  ( -1.540743955509788340E-33, -1.000000000000000000, -2.533398541561209262E-17 ) ) ;
#1889 = ADVANCED_FACE ( 'NONE', ( #4299 ), #1924, .F. ) ;
#1890 = ADVANCED_FACE ( 'NONE', ( #10319 ), #15948, .T. ) ;
#1891 = CARTESIAN_POINT ( 'NONE',  ( 0.3137051932979792457, -3.805684345189695783, -13.20008686438109891 ) ) ;
#1892 = ADVANCED_FACE ( 'NONE', ( #11377 ), #3862, .F. ) ;
#1893 = CONICAL_SURFACE ( 'NONE', #9208, 14.54644660717763927, 0.8559913436420816257 ) ;
#1894 = DIRECTION ( 'NONE',  ( -0.000000000000000000, -1.000000000000000000, 0.000000000000000000 ) ) ;
#1895 = CARTESIAN_POINT ( 'NONE',  ( 3.950837973638676281, 2.591948120962007884, -14.31366178983250670 ) ) ;
#1896 = CARTESIAN_POINT ( 'NONE',  ( 0.3150686449036038117, 8.199336701264542171, 11.02450593298021175 ) ) ;
#1897 = DIRECTION ( 'NONE',  ( 0.000000000000000000, -1.000000000000000000, 0.000000000000000000 ) ) ;
#1898 = CARTESIAN_POINT ( 'NONE',  ( -33.49999999999999289, -12.50000000000000178, -0.5000000000000000000 ) ) ;
#1899 = DIRECTION ( 'NONE',  ( 0.000000000000000000, 0.000000000000000000, 1.000000000000000000 ) ) ;
#1900 = CARTESIAN_POINT ( 'NONE',  ( 1.846613052777650976, 7.585914669018171352, 9.862487290071024759 ) ) ;
#1901 = ORIENTED_EDGE ( 'NONE', *, *, #12678, .F. ) ;
#1902 = VERTEX_POINT ( 'NONE', #1430 ) ;
#1903 = ORIENTED_EDGE ( 'NONE', *, *, #8948, .T. ) ;
#1904 = ORIENTED_EDGE ( 'NONE', *, *, #12004, .T. ) ;
#1905 = CARTESIAN_POINT ( 'NONE',  ( -5.000000000000000888, 17.00000000000000000, 8.000000000000000000 ) ) ;
#1906 = DIRECTION ( 'NONE',  ( 0.000000000000000000, 0.000000000000000000, 1.000000000000000000 ) ) ;
#1907 = CARTESIAN_POINT ( 'NONE',  ( 2.636624412717099908, 15.80357026013547816, -2.862162146981609201 ) ) ;
#1908 = CARTESIAN_POINT ( 'NONE',  ( 16.56822296793089322, 0.003834730849370841625, -0.009385634690641637967 ) ) ;
#1909 = CIRCLE ( 'NONE', #18376, 2.499999999999995115 ) ;
#1910 = CARTESIAN_POINT ( 'NONE',  ( 3.512766787570925864, 13.25664064834466593, -7.127386085302575225 ) ) ;
#1911 = ORIENTED_EDGE ( 'NONE', *, *, #824, .F. ) ;
#1912 = EDGE_CURVE ( 'NONE', #15844, #11944, #5028, .T. ) ;
#1913 = CARTESIAN_POINT ( 'NONE',  ( 4.447775431366602916, 7.499999999999999112, -16.63307795419225599 ) ) ;
#1914 = EDGE_CURVE ( 'NONE', #7670, #5120, #11272, .T. ) ;
#1915 = CARTESIAN_POINT ( 'NONE',  ( 3.686287386450715076E-15, -16.60000000000000142, 27.11316734529526329 ) ) ;
#1916 = EDGE_CURVE ( 'NONE', #17275, #15858, #8409, .T. ) ;
#1917 = DIRECTION ( 'NONE',  ( 0.000000000000000000, 0.000000000000000000, 1.000000000000000000 ) ) ;
#1918 = CARTESIAN_POINT ( 'NONE',  ( 1.847168016377980670, -9.955470380986684020, 7.464000291196382086 ) ) ;
#1919 = EDGE_CURVE ( 'NONE', #7625, #1518, #14240, .T. ) ;
#1920 = CARTESIAN_POINT ( 'NONE',  ( -5.000000000000000888, 17.00000000000000000, 8.000000000000000000 ) ) ;
#1921 = CARTESIAN_POINT ( 'NONE',  ( 0.3150686449036101955, 13.11344473514187925, 4.099563462784696632 ) ) ;
#1922 = B_SPLINE_CURVE_WITH_KNOTS ( 'NONE', 3,
 ( #18737, #2581, #1252, #15875, #17121, #4029 ),
 .UNSPECIFIED., .F., .F.,
 ( 4, 2, 4 ),
 ( 0.000000000000000000, 0.001657017934711440188, 0.003314035869422880375 ),
 .UNSPECIFIED. ) ;
#1923 =( BOUNDED_SURFACE ( )  B_SPLINE_SURFACE ( 3, 2, ( 
 ( #16150, #10412, #97 ),
 ( #11754, #16248, #3130 ),
 ( #14806, #7566, #290 ),
 ( #852, #10803, #14034 ),
 ( #8216, #5147, #583 ),
 ( #6311, #8126, #12146 ),
 ( #3530, #6408, #15461 ),
 ( #16725, #17976, #4880 ),
 ( #759, #10708, #6688 ),
 ( #7950, #3625, #16544 ),
 ( #9461, #3806, #3429 ),
 ( #671, #15283, #9266 ),
 ( #8035, #2276, #7850 ),
 ( #15370, #18249, #15096 ),
 ( #18332, #13936, #2014 ),
 ( #11085, #2194, #12502 ),
 ( #13670, #5241, #18153 ),
 ( #10904, #13843, #2369 ),
 ( #12239, #16900, #9634 ),
 ( #18063, #4968, #13756 ),
 ( #16629, #9365, #15197 ),
 ( #2110, #6500, #16811 ),
 ( #12323, #5055, #6592 ),
 ( #12416, #10995, #3715 ),
 ( #9542, #8389, #16998 ),
 ( #18419, #10101, #17362 ),
 ( #1211, #3903, #5691 ),
 ( #1305, #6967, #2728 ),
 ( #8573, #2639, #7149 ),
 ( #12867, #14313, #9907 ),
 ( #12778, #10002, #7056 ),
 ( #5423, #17087, #14220 ),
 ( #4278, #6779, #15737 ),
 ( #18694, #18515, #4188 ),
 ( #11543, #14397, #8483 ),
 ( #2451, #5596, #11447 ),
 ( #12686, #18604, #15834 ),
 ( #2539, #12962, #17265 ),
 ( #6865, #15927, #8302 ),
 ( #11270, #18793, #3992 ),
 ( #8662, #15637, #2816 ),
 ( #938, #12589, #1116 ),
 ( #5332, #11176, #5507 ),
 ( #9727, #15554, #14116 ) ),
 .UNSPECIFIED., .F., .F., .T. ) 
 B_SPLINE_SURFACE_WITH_KNOTS ( ( 4, 2, 2, 2, 2, 2, 2, 2, 2, 2, 2, 2, 2, 2, 2, 2, 2, 2, 2, 2, 2, 4 ),
 ( 3, 3 ),
 ( 0.007984881688765545563, 0.008880023643941227507, 0.009775165599116911186, 0.01067030755429259313, 0.01156544950946827507, 0.01246059146464395875, 0.01335573341981964070, 0.01425087537499532264, 0.01469844635258316448, 0.01492223184137708540, 0.01514601733017100632, 0.01536980281896492724, 0.01559358830775884816, 0.01581737379655277081, 0.01604115928534669000, 0.01693630124052237021, 0.01783144319569805042, 0.01872658515087373410, 0.01962172710604941778, 0.02051686906122510146, 0.02141201101640078513, 0.02230715297157646534 ),
 ( 0.000000000000000000, 1.000000000000000000 ),
 .UNSPECIFIED. ) 
 GEOMETRIC_REPRESENTATION_ITEM ( )  RATIONAL_B_SPLINE_SURFACE ( (
 ( 1.000000000000000000, 0.7071067811865475727, 1.000000000000000000),
 ( 1.000000000000000000, 0.7141735847352902455, 1.000000000000000000),
 ( 1.000000000000000000, 0.7220150969519002482, 1.000000000000000000),
 ( 1.000000000000000000, 0.7390483610380570445, 1.000000000000000000),
 ( 1.000000000000000000, 0.7482852340372653233, 1.000000000000000000),
 ( 1.000000000000000000, 0.7685052920442022595, 1.000000000000000000),
 ( 1.000000000000000000, 0.7795547470751481578, 1.000000000000000000),
 ( 1.000000000000000000, 0.8031735375541687594, 1.000000000000000000),
 ( 1.000000000000000000, 0.8157770400072592576, 1.000000000000000000),
 ( 1.000000000000000000, 0.8424364036431745140, 1.000000000000000000),
 ( 1.000000000000000000, 0.8565278543580376880, 1.000000000000000000),
 ( 1.000000000000000000, 0.8853337094944713215, 1.000000000000000000),
 ( 1.000000000000000000, 0.9000757013528374317, 1.000000000000000000),
 ( 1.000000000000000000, 0.9285356150545359677, 1.000000000000000000),
 ( 1.000000000000000000, 0.9423225300521840264, 1.000000000000000000),
 ( 1.000000000000000000, 0.9592421851076505801, 1.000000000000000000),
 ( 1.000000000000000000, 0.9642414584271785660, 1.000000000000000000),
 ( 1.000000000000000000, 0.9699277023943811971, 1.000000000000000000),
 ( 1.000000000000000000, 0.9715166551480145518, 1.000000000000000000),
 ( 1.000000000000000000, 0.9737696706145044789, 1.000000000000000000),
 ( 1.000000000000000000, 0.9744508395083761876, 1.000000000000000000),
 ( 1.000000000000000000, 0.9748110790397204184, 1.000000000000000000),
 ( 1.000000000000000000, 0.9744748476087129463, 1.000000000000000000),
 ( 1.000000000000000000, 0.9728601655991754305, 1.000000000000000000),
 ( 1.000000000000000000, 0.9715893508620192520, 1.000000000000000000),
 ( 1.000000000000000000, 0.9682746065025277238, 1.000000000000000000),
 ( 1.000000000000000000, 0.9662330922797167654, 1.000000000000000000),
 ( 1.000000000000000000, 0.9616633680012457441, 1.000000000000000000),
 ( 1.000000000000000000, 0.9591230388079776681, 1.000000000000000000),
 ( 1.000000000000000000, 0.9454866025348932501, 1.000000000000000000),
 ( 1.000000000000000000, 0.9317605398179132914, 1.000000000000000000),
 ( 1.000000000000000000, 0.9032287473899339725, 1.000000000000000000),
 ( 1.000000000000000000, 0.8883390392773735655, 1.000000000000000000),
 ( 1.000000000000000000, 0.8592388025803160412, 1.000000000000000000),
 ( 1.000000000000000000, 0.8450030273492536992, 1.000000000000000000),
 ( 1.000000000000000000, 0.8179255325836554125, 1.000000000000000000),
 ( 1.000000000000000000, 0.8050698650503534948, 1.000000000000000000),
 ( 1.000000000000000000, 0.7808988731588796250, 1.000000000000000000),
 ( 1.000000000000000000, 0.7696290231168499973, 1.000000000000000000),
 ( 1.000000000000000000, 0.7490294503509707935, 1.000000000000000000),
 ( 1.000000000000000000, 0.7396188834547036128, 1.000000000000000000),
 ( 1.000000000000000000, 0.7222670797466500536, 1.000000000000000000),
 ( 1.000000000000000000, 0.7142721232192589254, 1.000000000000000000),
 ( 1.000000000000000000, 0.7071067811865474617, 1.000000000000000000) ) ) 
 REPRESENTATION_ITEM ( '' )  SURFACE ( )  );
#1924 =( BOUNDED_SURFACE ( )  B_SPLINE_SURFACE ( 3, 1, ( 
 ( #7075, #17286 ),
 ( #16045, #2660 ),
 ( #5712, #4208 ),
 ( #2837, #7171 ) ),
 .UNSPECIFIED., .F., .F., .T. ) 
 B_SPLINE_SURFACE_WITH_KNOTS ( ( 4, 4 ),
 ( 2, 2 ),
 ( 0.000000000000000000, 1.000000000000000000 ),
 ( 0.000000000000000000, 1.000000000000000000 ),
 .UNSPECIFIED. ) 
 GEOMETRIC_REPRESENTATION_ITEM ( )  RATIONAL_B_SPLINE_SURFACE ( (
 ( 1.000000000000000000, 1.000000000000000000),
 ( 0.7792777138730160313, 0.9689936506012927220),
 ( 0.7792777138730160313, 0.9689936506012927220),
 ( 1.000000000000000000, 1.000000000000000000) ) ) 
 REPRESENTATION_ITEM ( '' )  SURFACE ( )  );
#1925 = ORIENTED_EDGE ( 'NONE', *, *, #9239, .T. ) ;
#1926 = B_SPLINE_CURVE_WITH_KNOTS ( 'NONE', 3,
 ( #2849, #14526, #4309, #6031, #16156, #13098 ),
 .UNSPECIFIED., .F., .F.,
 ( 4, 2, 4 ),
 ( 0.000000000000000000, 0.001656992708822557434, 0.003313985417645114867 ),
 .UNSPECIFIED. ) ;
#1927 = CARTESIAN_POINT ( 'NONE',  ( 1.254255976357533831, -13.61551404021209777, -5.487601330835152780 ) ) ;
#1929 = ORIENTED_EDGE ( 'NONE', *, *, #4337, .F. ) ;
#1928 = CARTESIAN_POINT ( 'NONE',  ( 25.00000000000000000, 7.499999999999999112, -17.00000000000000000 ) ) ;
#1930 = DIRECTION ( 'NONE',  ( 0.000000000000000000, 1.734723475976806700E-15, -1.000000000000000000 ) ) ;
#1931 = FACE_OUTER_BOUND ( 'NONE', #14603, .T. ) ;
#1932 = CIRCLE ( 'NONE', #10475, 5.000000000000000888 ) ;
#1933 = ORIENTED_EDGE ( 'NONE', *, *, #6009, .T. ) ;
#1934 = DIRECTION ( 'NONE',  ( -1.000000000000000000, -0.000000000000000000, -0.000000000000000000 ) ) ;
#1935 = CARTESIAN_POINT ( 'NONE',  ( 0.9490252293518500748, -6.938433416811018439, -12.00000000290481594 ) ) ;
#1936 = VERTEX_POINT ( 'NONE', #10025 ) ;
#1937 = CARTESIAN_POINT ( 'NONE',  ( 2.123976203522053297, -15.54801196254785722, -1.531817366691915483 ) ) ;
#1938 = CARTESIAN_POINT ( 'NONE',  ( 2.002547531651519996, 4.532360870844494016, -11.75462648437097180 ) ) ;
#1939 = DIRECTION ( 'NONE',  ( 1.000000000000000000, 0.000000000000000000, 0.000000000000000000 ) ) ;
#1940 = B_SPLINE_CURVE_WITH_KNOTS ( 'NONE', 3,
 ( #3691, #6667, #13821, #4948, #12480, #9246 ),
 .UNSPECIFIED., .F., .F.,
 ( 4, 2, 4 ),
 ( 4.192373019364431701E-17, 0.0002014099069817294621, 0.0004028198139634169657 ),
 .UNSPECIFIED. ) ;
#1941 = EDGE_CURVE ( 'NONE', #14610, #8961, #2571, .T. ) ;
#1942 = EDGE_LOOP ( 'NONE', ( #12597, #3775, #16274, #14695 ) ) ;
#1943 = CIRCLE ( 'NONE', #13220, 2.699999999999999734 ) ;
#1944 = CARTESIAN_POINT ( 'NONE',  ( 1.846955891736114852, -9.909315188408097441, 7.525208385419928092 ) ) ;
#1945 = FACE_OUTER_BOUND ( 'NONE', #8653, .T. ) ;
#1947 = ORIENTED_EDGE ( 'NONE', *, *, #6398, .T. ) ;
#1946 = CARTESIAN_POINT ( 'NONE',  ( 0.3137051932979792457, -11.37800749014136592, 7.698472063774431717 ) ) ;
#1948 = CARTESIAN_POINT ( 'NONE',  ( 3.950837973638675393, 10.05648675950126325, 10.51028938476221342 ) ) ;
#1949 = ORIENTED_EDGE ( 'NONE', *, *, #984, .T. ) ;
#1950 = CARTESIAN_POINT ( 'NONE',  ( 0.3142014840576534684, -4.608051180497015231, 12.94260032291127160 ) ) ;
#1951 = CARTESIAN_POINT ( 'NONE',  ( 2.697797270744666243, -13.26309265156976558, -0.9169917281808652731 ) ) ;
#1952 = ORIENTED_EDGE ( 'NONE', *, *, #15219, .F. ) ;
#1953 = ORIENTED_EDGE ( 'NONE', *, *, #15909, .T. ) ;
#1954 = FACE_OUTER_BOUND ( 'NONE', #12857, .T. ) ;
#1955 = ADVANCED_FACE ( 'NONE', ( #7366, #6988 ), #13178, .T. ) ;
#1956 = ORIENTED_EDGE ( 'NONE', *, *, #18463, .T. ) ;
#1957 = FACE_OUTER_BOUND ( 'NONE', #3513, .T. ) ;
#1958 = ORIENTED_EDGE ( 'NONE', *, *, #15429, .F. ) ;
#1960 = CARTESIAN_POINT ( 'NONE',  ( 2.636624412714236865, 0.000000000000000000, 0.000000000000000000 ) ) ;
#1959 = VECTOR ( 'NONE', #7017, 1000.000000000000000 ) ;
#1961 = CARTESIAN_POINT ( 'NONE',  ( 12.00000000000000711, -19.99999999999999645, 3.000000000000000000 ) ) ;
#1962 = CARTESIAN_POINT ( 'NONE',  ( 0.4862570985993235340, 10.79774104611385965, -8.769551628660616771 ) ) ;
#1963 = PLANE ( 'NONE',  #5380 ) ;
#1964 = CARTESIAN_POINT ( 'NONE',  ( 16.56872352241294521, -0.009207754980063714498, -0.004907101719994726684 ) ) ;
#1965 = CARTESIAN_POINT ( 'NONE',  ( 1.451356985208877954E-14, -9.013167318348349610, 16.24521815286417947 ) ) ;
#1966 = DIRECTION ( 'NONE',  ( 0.7635533937278214944, 0.6204116510013490959, -0.1790966170213899034 ) ) ;
#1967 = CARTESIAN_POINT ( 'NONE',  ( 2.002547531651519996, 10.57595306287302250, -6.845637710436074386 ) ) ;
#1968 = CARTESIAN_POINT ( 'NONE',  ( 2.636624412717140764, -2.862162146982851763, -15.80357026013259514 ) ) ;
#1969 = CARTESIAN_POINT ( 'NONE',  ( 0.3150692679895976678, 7.951395415075086959, 11.20465057551027854 ) ) ;
#1970 = CARTESIAN_POINT ( 'NONE',  ( 2.002547531651519996, -12.57989064830760206, 0.6781519942171299054 ) ) ;
#1971 = CIRCLE ( 'NONE', #3477, 5.000000000000000000 ) ;
#1972 = CARTESIAN_POINT ( 'NONE',  ( 2.636624412716062960, 6.973567714909310489, -14.46769361191320868 ) ) ;
#1973 =( NAMED_UNIT ( * ) SI_UNIT ( $, .STERADIAN. ) SOLID_ANGLE_UNIT ( ) );
#1974 = ORIENTED_EDGE ( 'NONE', *, *, #2782, .F. ) ;
#1975 = EDGE_CURVE ( 'NONE', #11815, #11886, #5621, .T. ) ;
#1976 = ORIENTED_EDGE ( 'NONE', *, *, #11935, .F. ) ;
#1977 = ORIENTED_EDGE ( 'NONE', *, *, #3834, .F. ) ;
#1978 = ORIENTED_EDGE ( 'NONE', *, *, #8575, .T. ) ;
#1979 = EDGE_CURVE ( 'NONE', #8074, #16551, #11037, .T. ) ;
#1980 = LINE ( 'NONE', #7820, #2247 ) ;
#1981 = CARTESIAN_POINT ( 'NONE',  ( 1.846138399168762101, 0.4167076046095548603, 12.43476674860266762 ) ) ;
#1982 = CARTESIAN_POINT ( 'NONE',  ( 1.845756295923360435, -7.694561132136879422, -9.776763338604684606 ) ) ;
#1983 = CARTESIAN_POINT ( 'NONE',  ( 3.950837973638668288, 14.41405733518061716, 1.958075594453843493 ) ) ;
#1984 = VECTOR ( 'NONE', #6709, 1000.000000000000000 ) ;
#1985 = DIRECTION ( 'NONE',  ( 1.000000000000000000, 0.000000000000000000, 0.000000000000000000 ) ) ;
#1986 = PRODUCT_DEFINITION_CONTEXT ( 'detailed design', #3750, 'design' ) ;
#1987 = CARTESIAN_POINT ( 'NONE',  ( 0.3137051932979757485, -11.37800749014125223, -7.698472063774596030 ) ) ;
#1988 = CARTESIAN_POINT ( 'NONE',  ( 1.560000000000000053, -0.8660254037844384856, -1.500000000000000000 ) ) ;
#1989 = CARTESIAN_POINT ( 'NONE',  ( 0.4754618798421162973, -8.775436892861190330, 10.80499583390509954 ) ) ;
#1990 = CARTESIAN_POINT ( 'NONE',  ( 0.000000000000000000, 0.000000000000000000, 0.000000000000000000 ) ) ;
#1991 = CARTESIAN_POINT ( 'NONE',  ( 1.846138399168762101, -11.69739621335919111, -4.238866729160527314 ) ) ;
#1992 = B_SPLINE_CURVE_WITH_KNOTS ( 'NONE', 3,
 ( #6535, #882, #6723, #2043, #18366, #5181 ),
 .UNSPECIFIED., .F., .F.,
 ( 4, 2, 4 ),
 ( 1.084202172485504434E-19, 0.0002017457492448070664, 0.0004034914984896140243 ),
 .UNSPECIFIED. ) ;
#1993 = CARTESIAN_POINT ( 'NONE',  ( 16.56753206892534891, 0.004368917149004243779, -0.008432171035096398468 ) ) ;
#1994 = VECTOR ( 'NONE', #1106, 1000.000000000000000 ) ;
#1995 = CARTESIAN_POINT ( 'NONE',  ( 16.57778382496167424, -0.006312874906843954532, -0.01354073047775891311 ) ) ;
#1996 = ORIENTED_EDGE ( 'NONE', *, *, #4691, .T. ) ;
#1997 =( BOUNDED_SURFACE ( )  B_SPLINE_SURFACE ( 3, 1, ( 
 ( #13516, #7993 ),
 ( #6548, #16402 ),
 ( #12369, #17930 ),
 ( #4925, #15048 ) ),
 .UNSPECIFIED., .F., .F., .T. ) 
 B_SPLINE_SURFACE_WITH_KNOTS ( ( 4, 4 ),
 ( 2, 2 ),
 ( 0.000000000000000000, 1.000000000000000000 ),
 ( 0.000000000000000000, 1.000000000000000000 ),
 .UNSPECIFIED. ) 
 GEOMETRIC_REPRESENTATION_ITEM ( )  RATIONAL_B_SPLINE_SURFACE ( (
 ( 1.000000000000000000, 1.000000000000000000),
 ( 0.9933953342250436691, 0.8357391271907733676),
 ( 0.9933953342250436691, 0.8357391271907733676),
 ( 1.000000000000000000, 1.000000000000000000) ) ) 
 REPRESENTATION_ITEM ( '' )  SURFACE ( )  );
#1998 = EDGE_CURVE ( 'NONE', #9992, #11554, #4191, .T. ) ;
#1999 = ORIENTED_EDGE ( 'NONE', *, *, #13858, .F. ) ;
#2000 = EDGE_CURVE ( 'NONE', #12695, #415, #12191, .T. ) ;
#2001 = ORIENTED_EDGE ( 'NONE', *, *, #18463, .F. ) ;
#2002 = CONICAL_SURFACE ( 'NONE', #9915, 14.54644660717763927, 0.8559913436420816257 ) ;
#2003 = EDGE_LOOP ( 'NONE', ( #7026, #3592, #14579 ) ) ;
#2004 = TOROIDAL_SURFACE ( 'NONE', #8710, 3.499999999999994671, 0.5000000000000000000 ) ;
#2005 = CARTESIAN_POINT ( 'NONE',  ( 8.522092701127531811, -5.397361180353174248, 4.388629235579559307 ) ) ;
#2006 = VECTOR ( 'NONE', #13244, 1000.000000000000000 ) ;
#2007 = CARTESIAN_POINT ( 'NONE',  ( 2.636624412714236865, 0.000000000000000000, 0.000000000000000000 ) ) ;
#2008 = DIRECTION ( 'NONE',  ( -1.000000000000000000, 0.000000000000000000, 0.000000000000000000 ) ) ;
#2009 = LINE ( 'NONE', #7558, #8984 ) ;
#2010 = CARTESIAN_POINT ( 'NONE',  ( 2.636624412716913390, 14.14563173255587536, -7.605649742760633991 ) ) ;
#2011 = ORIENTED_EDGE ( 'NONE', *, *, #318, .F. ) ;
#2012 = CARTESIAN_POINT ( 'NONE',  ( -5.342326914280422834, 7.500000000000000000, -16.88455910646440827 ) ) ;
#2013 = FACE_OUTER_BOUND ( 'NONE', #6659, .T. ) ;
#2014 = CARTESIAN_POINT ( 'NONE',  ( -1.149093537842120316, 7.499999999999999112, -14.62468756229416300 ) ) ;
#2015 = CARTESIAN_POINT ( 'NONE',  ( 0.000000000000000000, 0.000000000000000000, -14.50215154756889824 ) ) ;
#2016 = CARTESIAN_POINT ( 'NONE',  ( 18.75000000000000000, 2.516649172247811061E-16, -2.055000000000000160 ) ) ;
#2017 = SURFACE_STYLE_USAGE ( .BOTH. , #16547 ) ;
#2018 = CARTESIAN_POINT ( 'NONE',  ( 1.846138399168762101, 0.4167076046097279440, -12.43476674860266051 ) ) ;
#2019 = ORIENTED_EDGE ( 'NONE', *, *, #8392, .T. ) ;
#2020 = CARTESIAN_POINT ( 'NONE',  ( 0.4862570985993235340, -10.79774104611379215, 8.769551628660700260 ) ) ;
#2022 = ORIENTED_EDGE ( 'NONE', *, *, #5052, .T. ) ;
#2021 = CARTESIAN_POINT ( 'NONE',  ( 1.846822687350019754, 11.92063725419904152, -3.566003975885565946 ) ) ;
#2023 = CARTESIAN_POINT ( 'NONE',  ( -997.5739745962155212, 0.000000000000000000, 0.000000000000000000 ) ) ;
#2024 = EDGE_CURVE ( 'NONE', #913, #1072, #14198, .T. ) ;
#2025 = EDGE_CURVE ( 'NONE', #18618, #16284, #1815, .T. ) ;
#2026 = ORIENTED_EDGE ( 'NONE', *, *, #9182, .F. ) ;
#2027 = DIRECTION ( 'NONE',  ( -1.000000000000000000, 0.000000000000000000, 0.000000000000000000 ) ) ;
#2028 = VECTOR ( 'NONE', #14678, 1000.000000000000000 ) ;
#2029 = CARTESIAN_POINT ( 'NONE',  ( -4.162578369387166077, -7.500000000000000888, -16.52352554129683426 ) ) ;
#2030 = AXIS2_PLACEMENT_3D ( 'NONE', #15716, #11248, #17249 ) ;
#2031 = ORIENTED_EDGE ( 'NONE', *, *, #4741, .F. ) ;
#2032 = CARTESIAN_POINT ( 'NONE',  ( 8.522092701127531811, 3.777034505568607425, -5.841710761610089619 ) ) ;
#2033 = AXIS2_PLACEMENT_3D ( 'NONE', #8613, #9948, #12 ) ;
#2034 = CARTESIAN_POINT ( 'NONE',  ( 0.3150686449036029790, 13.73846184595214304, -0.1533607327086227434 ) ) ;
#2035 = DIRECTION ( 'NONE',  ( 1.000000000000000000, -0.000000000000000000, 0.000000000000000000 ) ) ;
#2036 = LINE ( 'NONE', #692, #12375 ) ;
#2037 = CARTESIAN_POINT ( 'NONE',  ( 1.845756295923360657, -6.920504327368265152, 10.33914852636102033 ) ) ;
#2038 = DIRECTION ( 'NONE',  ( -1.000000000000000000, 0.000000000000000000, 0.000000000000000000 ) ) ;
#2040 = ORIENTED_EDGE ( 'NONE', *, *, #15270, .T. ) ;
#2039 = CARTESIAN_POINT ( 'NONE',  ( 0.3308579732647032867, -11.46737410776358779, 7.595989242675092790 ) ) ;
#2041 = CARTESIAN_POINT ( 'NONE',  ( 3.074695600507254767, -11.23985886659442635, 10.75417554975694578 ) ) ;
#2042 = B_SPLINE_CURVE_WITH_KNOTS ( 'NONE', 3,
 ( #17812, #5941, #4527, #4716, #3837, #4991 ),
 .UNSPECIFIED., .F., .F.,
 ( 4, 2, 4 ),
 ( 1.084202172485504434E-19, 0.001657017934709843158, 0.003314035869419686316 ),
 .UNSPECIFIED. ) ;
#2043 = CARTESIAN_POINT ( 'NONE',  ( 0.3939875929385636688, 8.678227324501120776, 10.75308190953746212 ) ) ;
#2044 = CARTESIAN_POINT ( 'NONE',  ( 2.002547531651519996, -12.57989064830759141, -0.6781519942173057647 ) ) ;
#2045 = ORIENTED_EDGE ( 'NONE', *, *, #16190, .T. ) ;
#2046 = ORIENTED_EDGE ( 'NONE', *, *, #7348, .F. ) ;
#2047 = DIRECTION ( 'NONE',  ( -0.4246593920385851040, -0.1376957914266804250, 0.8948208031649687033 ) ) ;
#2048 = EDGE_CURVE ( 'NONE', #17649, #12162, #91, .T. ) ;
#2049 = AXIS2_PLACEMENT_3D ( 'NONE', #17593, #1444, #9087 ) ;
#2050 = VERTEX_POINT ( 'NONE', #936 ) ;
#2051 = DIRECTION ( 'NONE',  ( 0.000000000000000000, 0.000000000000000000, 1.000000000000000000 ) ) ;
#2052 = ADVANCED_FACE ( 'NONE', ( #10902 ), #12402, .F. ) ;
#2053 = ORIENTED_EDGE ( 'NONE', *, *, #4035, .F. ) ;
#2054 = VECTOR ( 'NONE', #11619, 1000.000000000000000 ) ;
#2055 = CARTESIAN_POINT ( 'NONE',  ( 16.56753206892534891, -0.006669401563385243120, -0.006760771273035091553 ) ) ;
#2056 = VECTOR ( 'NONE', #6749, 1000.000000000000227 ) ;
#2057 = CARTESIAN_POINT ( 'NONE',  ( 3.512766787571172333, 14.91422000116773994, 2.025881399556380469 ) ) ;
#2058 = CARTESIAN_POINT ( 'NONE',  ( 25.00000000000000000, 2.499999999999997780, -17.00000000000000000 ) ) ;
#2059 = DIRECTION ( 'NONE',  ( 0.000000000000000000, 0.000000000000000000, -1.000000000000000000 ) ) ;
#2060 = DIRECTION ( 'NONE',  ( -1.224646799147353207E-16, 1.000000000000000000, 0.000000000000000000 ) ) ;
#2061 = AXIS2_PLACEMENT_3D ( 'NONE', #12590, #2277, #3626 ) ;
#2062 = EDGE_CURVE ( 'NONE', #10419, #14675, #774, .T. ) ;
#2063 = CONICAL_SURFACE ( 'NONE', #15181, 1732.050807568857181, 1.047197551196592746 ) ;
#2064 = CARTESIAN_POINT ( 'NONE',  ( 0.3142014840576501378, -0.3830336514509840029, 13.73311050063163918 ) ) ;
#2065 = CARTESIAN_POINT ( 'NONE',  ( 8.438534575730034959, -3.845978796786076348, 5.688336279099031501 ) ) ;
#2066 = PRESENTATION_STYLE_ASSIGNMENT (( #435 ) ) ;
#2067 = CARTESIAN_POINT ( 'NONE',  ( 0.4754618798421162973, -5.007009103465343003, 12.98792082933642789 ) ) ;
#2068 = CARTESIAN_POINT ( 'NONE',  ( 0.4385251269669946939, -11.63205320541528209, 7.540955776459703053 ) ) ;
#2069 = VECTOR ( 'NONE', #815, 1000.000000000000000 ) ;
#2070 = CARTESIAN_POINT ( 'NONE',  ( 16.56822296793089322, -0.0007467251401289379167, 0.01011126603341003759 ) ) ;
#2071 = CONICAL_SURFACE ( 'NONE', #231, 14.54644660717763927, 0.8559913436420816257 ) ;
#2072 = CARTESIAN_POINT ( 'NONE',  ( 2.636624412715138366, -15.91454522070249311, -2.161493821597819665 ) ) ;
#2073 = PRODUCT_DEFINITION ( 'UNKNOWN', '', #9290, #10776 ) ;
#2074 = CARTESIAN_POINT ( 'NONE',  ( 1.861706995891676764, 12.44571539481144384, -0.5394761475746276957 ) ) ;
#2075 = LINE ( 'NONE', #10866, #2056 ) ;
#2076 = EDGE_CURVE ( 'NONE', #11529, #3979, #12319, .T. ) ;
#2077 = EDGE_LOOP ( 'NONE', ( #13785, #14387, #12473, #3682 ) ) ;
#2078 = ORIENTED_EDGE ( 'NONE', *, *, #17877, .T. ) ;
#2079 = EDGE_CURVE ( 'NONE', #14201, #447, #9442, .T. ) ;
#2080 = ORIENTED_EDGE ( 'NONE', *, *, #2600, .F. ) ;
#2081 = ADVANCED_FACE ( 'NONE', ( #15550 ), #11074, .F. ) ;
#2082 = ORIENTED_EDGE ( 'NONE', *, *, #1532, .F. ) ;
#2083 = ORIENTED_EDGE ( 'NONE', *, *, #6251, .T. ) ;
#2084 = CONICAL_SURFACE ( 'NONE', #18539, 12.50000000000000355, 1.308996938995747428 ) ;
#2085 = CARTESIAN_POINT ( 'NONE',  ( 15.00000000000000711, -15.99999999999999645, 7.000000000000000000 ) ) ;
#2086 = CARTESIAN_POINT ( 'NONE',  ( -6.538348415311014072, -7.500000000000000888, -16.99999999999999645 ) ) ;
#2087 = CARTESIAN_POINT ( 'NONE',  ( 3.377929128793393687, 12.02809354424100619, 7.136734442940879219 ) ) ;
#2088 = CARTESIAN_POINT ( 'NONE',  ( -6.538348415311014072, 7.499999999999999112, -16.99999999999999645 ) ) ;
#2089 = CARTESIAN_POINT ( 'NONE',  ( 2.636624412715999011, 2.161493821598055920, -15.91454522070273647 ) ) ;
#2090 = EDGE_CURVE ( 'NONE', #8004, #6249, #5102, .T. ) ;
#2091 = CARTESIAN_POINT ( 'NONE',  ( 16.58200780006414732, 0.007066318000004704822, 0.008650561019685554590 ) ) ;
#2092 = CARTESIAN_POINT ( 'NONE',  ( 0.3720661004400040439, 10.73619472937714825, -8.694226082900476271 ) ) ;
#2093 = CARTESIAN_POINT ( 'NONE',  ( 20.00000000000000000, -2.500000000000000444, -17.00000000000000000 ) ) ;
#2094 = CARTESIAN_POINT ( 'NONE',  ( 3.353306896162455697, 3.007732942432417289, 13.62210141459496171 ) ) ;
#2095 = AXIS2_PLACEMENT_3D ( 'NONE', #13304, #6051, #11878 ) ;
#2096 = VERTEX_POINT ( 'NONE', #16897 ) ;
#2097 = EDGE_LOOP ( 'NONE', ( #13783, #6508, #11629, #2309 ) ) ;
#2098 = ORIENTED_EDGE ( 'NONE', *, *, #10946, .T. ) ;
#2099 = VERTEX_POINT ( 'NONE', #6590 ) ;
#2100 = CARTESIAN_POINT ( 'NONE',  ( 1.560000000000000053, 1.299038105676658228, -0.7500000000000009992 ) ) ;
#2101 = CIRCLE ( 'NONE', #14295, 5.000000000000000000 ) ;
#2102 = DIRECTION ( 'NONE',  ( 0.000000000000000000, 0.000000000000000000, 1.000000000000000000 ) ) ;
#2103 = CARTESIAN_POINT ( 'NONE',  ( 1.847461586945729595, -7.341074796295863791, -10.04711372545053116 ) ) ;
#2104 = CARTESIAN_POINT ( 'NONE',  ( 2.747332970342022840, -14.49942876448597673, 7.555624153089596895 ) ) ;
#2105 = DIRECTION ( 'NONE',  ( 1.000000000000000000, 0.000000000000000000, 0.000000000000000000 ) ) ;
#2106 = VERTEX_POINT ( 'NONE', #9540 ) ;
#2107 = CARTESIAN_POINT ( 'NONE',  ( 1.959212340397967766, -0.6675998551412658522, 12.53706137681888677 ) ) ;
#2108 = ADVANCED_FACE ( 'NONE', ( #5051 ), #5798, .F. ) ;
#2109 = CARTESIAN_POINT ( 'NONE',  ( 0.4754618798421167414, -13.45049478164062329, 3.583352865732619463 ) ) ;
#2110 = CARTESIAN_POINT ( 'NONE',  ( 0.09864563712547316787, 7.002566078024234919, -11.99999999788117044 ) ) ;
#2111 = FACE_OUTER_BOUND ( 'NONE', #10163, .T. ) ;
#2112 = ADVANCED_FACE ( 'NONE', ( #18885 ), #7343, .T. ) ;
#2113 =( LENGTH_UNIT ( ) NAMED_UNIT ( * ) SI_UNIT ( .MILLI., .METRE. ) );
#2114 = DIRECTION ( 'NONE',  ( 0.000000000000000000, 0.000000000000000000, -1.000000000000000000 ) ) ;
#2115 =( BOUNDED_SURFACE ( )  B_SPLINE_SURFACE ( 3, 1, ( 
 ( #8381, #6856 ),
 ( #7050, #3707 ),
 ( #12770, #2445 ),
 ( #8295, #14110 ) ),
 .UNSPECIFIED., .F., .F., .T. ) 
 B_SPLINE_SURFACE_WITH_KNOTS ( ( 4, 4 ),
 ( 2, 2 ),
 ( 0.000000000000000000, 1.000000000000000000 ),
 ( 0.000000000000000000, 1.000000000000000000 ),
 .UNSPECIFIED. ) 
 GEOMETRIC_REPRESENTATION_ITEM ( )  RATIONAL_B_SPLINE_SURFACE ( (
 ( 1.000000000000000000, 1.000000000000000000),
 ( 0.9933953342250436691, 0.8357391271907733676),
 ( 0.9933953342250436691, 0.8357391271907733676),
 ( 1.000000000000000000, 1.000000000000000000) ) ) 
 REPRESENTATION_ITEM ( '' )  SURFACE ( )  );
#2116 = ORIENTED_EDGE ( 'NONE', *, *, #13575, .T. ) ;
#2118 = ORIENTED_EDGE ( 'NONE', *, *, #9241, .T. ) ;
#2117 = CARTESIAN_POINT ( 'NONE',  ( 1.342453679581834924, -11.38190519890860131, 9.456403821038760427 ) ) ;
#2119 = CARTESIAN_POINT ( 'NONE',  ( 1.861706995891668104, 12.00328602385080679, 3.332865258614018611 ) ) ;
#2120 = VERTEX_POINT ( 'NONE', #11630 ) ;
#2121 = CARTESIAN_POINT ( 'NONE',  ( 1.959283090834840646, -4.509128209890892691, -11.71721539537259282 ) ) ;
#2122 = CARTESIAN_POINT ( 'NONE',  ( -2.061733300930191692, -7.500000000000532019, -13.14107379030518530 ) ) ;
#2123 = ORIENTED_EDGE ( 'NONE', *, *, #17662, .T. ) ;
#2124 = CARTESIAN_POINT ( 'NONE',  ( 2.697797270744666243, 8.537712152181008207, -10.19107313879048249 ) ) ;
#2125 = CARTESIAN_POINT ( 'NONE',  ( 0.4754618798421162973, 13.89949764182682657, -0.7484603771384912285 ) ) ;
#2126 = CARTESIAN_POINT ( 'NONE',  ( 1.845756295923359769, -11.97166802574123423, -3.386818134580184658 ) ) ;
#2127 = CARTESIAN_POINT ( 'NONE',  ( 0.8740764193766140666, 14.27348595579769253, 0.8420116711621705718 ) ) ;
#2128 = EDGE_CURVE ( 'NONE', #9839, #9866, #16275, .T. ) ;
#2129 = EDGE_CURVE ( 'NONE', #18838, #8358, #15102, .T. ) ;
#2130 = ADVANCED_FACE ( 'NONE', ( #13153 ), #17459, .T. ) ;
#2131 = CIRCLE ( 'NONE', #14618, 7.000000000000000000 ) ;
#2132 = PRESENTATION_LAYER_ASSIGNMENT (  '', '', ( #5469 ) ) ;
#2133 = FILL_AREA_STYLE_COLOUR ( '', #11487 ) ;
#2134 = CARTESIAN_POINT ( 'NONE',  ( 2.747332970342022840, -16.12459247543624130, -2.705255688518015234 ) ) ;
#2135 = DIRECTION ( 'NONE',  ( -1.000000000000000000, -0.000000000000000000, -0.000000000000000000 ) ) ;
#2137 = VERTEX_POINT ( 'NONE', #1403 ) ;
#2136 = CARTESIAN_POINT ( 'NONE',  ( 1.918921323896323639, 10.48468902844562578, -6.832782632379261756 ) ) ;
#2138 = DIRECTION ( 'NONE',  ( 0.000000000000000000, 0.000000000000000000, 1.000000000000000000 ) ) ;
#2139 = CONICAL_SURFACE ( 'NONE', #12208, 16.06066017081991149, 0.7853981625000062694 ) ;
#2140 = ORIENTED_EDGE ( 'NONE', *, *, #18386, .T. ) ;
#2141 = CARTESIAN_POINT ( 'NONE',  ( 16.56872352241294521, -0.007512283835804365630, 0.007240717549633862542 ) ) ;
#2142 = DIRECTION ( 'NONE',  ( 0.000000000000000000, 0.000000000000000000, -1.000000000000000000 ) ) ;
#2143 = EDGE_CURVE ( 'NONE', #11376, #2137, #1678, .T. ) ;
#2144 = ORIENTED_EDGE ( 'NONE', *, *, #17987, .F. ) ;
#2145 = ORIENTED_EDGE ( 'NONE', *, *, #15651, .T. ) ;
#2146 = DIRECTION ( 'NONE',  ( 0.000000000000000000, 0.000000000000000000, 1.000000000000000000 ) ) ;
#2147 = LINE ( 'NONE', #7984, #18677 ) ;
#2148 = VERTEX_POINT ( 'NONE', #4366 ) ;
#2149 = CARTESIAN_POINT ( 'NONE',  ( -194.9999999999999716, -10.00000000000002665, 5.999999999999999112 ) ) ;
#2150 = CARTESIAN_POINT ( 'NONE',  ( -30.00000000000000355, -12.50000000000000178, 0.000000000000000000 ) ) ;
#2151 = CARTESIAN_POINT ( 'NONE',  ( 3.950837973638675393, 6.888253895133479965, -12.81214529934967672 ) ) ;
#2152 = CARTESIAN_POINT ( 'NONE',  ( 16.57210152137263393, 0.01214401161737623663, 0.008007331252333469568 ) ) ;
#2153 = PRODUCT_CONTEXT ( 'NONE', #3119, 'mechanical' ) ;
#2154 = ADVANCED_FACE ( 'NONE', ( #4081 ), #1209, .T. ) ;
#2155 =( NAMED_UNIT ( * ) PLANE_ANGLE_UNIT ( ) SI_UNIT ( $, .RADIAN. ) );
#2156 = CARTESIAN_POINT ( 'NONE',  ( 16.56782317627811096, -0.009228812961908680612, 0.003357783021327786360 ) ) ;
#2157 = CARTESIAN_POINT ( 'NONE',  ( 1.846138399168762101, 3.446241763653166590, -11.95493567637846866 ) ) ;
#2158 = ADVANCED_FACE ( 'NONE', ( #18791 ), #2563, .T. ) ;
#2159 = CARTESIAN_POINT ( 'NONE',  ( 16.56872352241294521, 0.009207754980063749192, 0.004907101719994666836 ) ) ;
#2160 = CYLINDRICAL_SURFACE ( 'NONE', #10914, 2.600000000000039613 ) ;
#2161 = DIRECTION ( 'NONE',  ( 0.000000000000000000, 0.000000000000000000, -1.000000000000000000 ) ) ;
#2162 = PRESENTATION_STYLE_ASSIGNMENT (( #3391 ) ) ;
#2163 = ORIENTED_EDGE ( 'NONE', *, *, #12769, .F. ) ;
#2164 = ADVANCED_FACE ( 'NONE', ( #8660, #4276 ), #16018, .T. ) ;
#2165 = ORIENTED_EDGE ( 'NONE', *, *, #17163, .T. ) ;
#2166 = ORIENTED_EDGE ( 'NONE', *, *, #8213, .T. ) ;
#2167 = ORIENTED_EDGE ( 'NONE', *, *, #4053, .T. ) ;
#2168 = ORIENTED_EDGE ( 'NONE', *, *, #8921, .F. ) ;
#2169 = LINE ( 'NONE', #16970, #15447 ) ;
#2170 = CARTESIAN_POINT ( 'NONE',  ( 0.3308579732647040639, 4.812490080619379995, -12.88563776947740358 ) ) ;
#2171 = ORIENTED_EDGE ( 'NONE', *, *, #3888, .T. ) ;
#2172 = CARTESIAN_POINT ( 'NONE',  ( 16.56872352241294521, -0.01033355228142500762, -0.001442253899401184716 ) ) ;
#2173 = CARTESIAN_POINT ( 'NONE',  ( 1.847461586945728929, -11.82388984758122064, 3.877048136045332605 ) ) ;
#2174 = DIRECTION ( 'NONE',  ( -0.000000000000000000, 1.000000000000000000, -0.000000000000000000 ) ) ;
#2175 = CARTESIAN_POINT ( 'NONE',  ( 2.353870697619111496, -10.90705766126224674, 6.980654702310806314 ) ) ;
#2176 = CARTESIAN_POINT ( 'NONE',  ( 3.377929128793398128, -13.64476897106782083, -3.070552481925011179 ) ) ;
#2177 = ADVANCED_FACE ( 'NONE', ( #9904 ), #7787, .F. ) ;
#2178 = CARTESIAN_POINT ( 'NONE',  ( 2.636624412715137034, -11.60464335004055947, 11.10302021257951743 ) ) ;
#2179 = CARTESIAN_POINT ( 'NONE',  ( 1.846138399168762101, 0.4167076046095548603, 12.43476674860266762 ) ) ;
#2180 = ORIENTED_EDGE ( 'NONE', *, *, #9576, .T. ) ;
#2181 = ORIENTED_EDGE ( 'NONE', *, *, #18056, .F. ) ;
#2182 = ORIENTED_EDGE ( 'NONE', *, *, #11569, .F. ) ;
#2183 = ORIENTED_EDGE ( 'NONE', *, *, #4663, .F. ) ;
#2184 = CARTESIAN_POINT ( 'NONE',  ( 1.254009781012409341, 13.61532727684501509, -5.487405433548977030 ) ) ;
#2185 = EDGE_CURVE ( 'NONE', #3512, #10137, #18159, .T. ) ;
#2186 = CARTESIAN_POINT ( 'NONE',  ( 5.000000000000000888, 17.00000000000000000, 4.000000000000000000 ) ) ;
#2187 = AXIS2_PLACEMENT_3D ( 'NONE', #103, #15959, #18829 ) ;
#2188 = FACE_OUTER_BOUND ( 'NONE', #16097, .T. ) ;
#2189 = CARTESIAN_POINT ( 'NONE',  ( 1.846822687350018866, 12.43915556955403900, 0.2922081769260583273 ) ) ;
#2190 = CARTESIAN_POINT ( 'NONE',  ( 0.4862570985993252548, 13.44146924561381162, 3.580942890621718888 ) ) ;
#2191 = ORIENTED_EDGE ( 'NONE', *, *, #18654, .F. ) ;
#2192 = CARTESIAN_POINT ( 'NONE',  ( 1.846138399168762101, -0.4167076046096411246, 12.43476674860266407 ) ) ;
#2193 = CARTESIAN_POINT ( 'NONE',  ( 8.522092701127531811, 5.841710761610131364, 3.777034505568545253 ) ) ;
#2194 = CARTESIAN_POINT ( 'NONE',  ( -1.461502493107204925, 7.500000000000000888, -13.09494173305782994 ) ) ;
#2195 = CARTESIAN_POINT ( 'NONE',  ( 0.4862570985993235340, 13.89016912371017476, 0.7479633556562934604 ) ) ;
#2196 = DIRECTION ( 'NONE',  ( 0.000000000000000000, 0.000000000000000000, 1.000000000000000000 ) ) ;
#2197 = CARTESIAN_POINT ( 'NONE',  ( 0.000000000000000000, 0.000000000000000000, 8.000000000000000000 ) ) ;
#2198 = CARTESIAN_POINT ( 'NONE',  ( 0.4862570985993235340, 11.67702470553376060, -7.559321496869298329 ) ) ;
#2199 = LINE ( 'NONE', #16475, #8487 ) ;
#2200 = ORIENTED_EDGE ( 'NONE', *, *, #5215, .F. ) ;
#2202 = ORIENTED_EDGE ( 'NONE', *, *, #15444, .T. ) ;
#2201 = LINE ( 'NONE', #677, #9660 ) ;
#2203 = CARTESIAN_POINT ( 'NONE',  ( 0.4754618798421171855, 13.45049478164060019, 3.583352865732718495 ) ) ;
#2204 = ADVANCED_FACE ( 'NONE', ( #17170 ), #15734, .T. ) ;
#2205 = VECTOR ( 'NONE', #1158, 1000.000000000000000 ) ;
#2206 = EDGE_CURVE ( 'NONE', #6765, #5117, #17416, .T. ) ;
#2207 = ORIENTED_EDGE ( 'NONE', *, *, #12285, .T. ) ;
#2208 = CARTESIAN_POINT ( 'NONE',  ( 16.56753206892534891, -0.004253784598196824578, -0.008490833999797990639 ) ) ;
#2209 = CARTESIAN_POINT ( 'NONE',  ( -1.870513085853194424, -6.747912118474371113, -12.00000000532778266 ) ) ;
#2210 = ORIENTED_EDGE ( 'NONE', *, *, #8999, .T. ) ;
#2211 = CARTESIAN_POINT ( 'NONE',  ( 1.846613052777651198, -7.035606253495386930, 10.26230975746757146 ) ) ;
#2212 = CARTESIAN_POINT ( 'NONE',  ( 2.705023505549863039, 3.294610156756076602, -12.88681800078729189 ) ) ;
#2213 = CYLINDRICAL_SURFACE ( 'NONE', #13097, 10.00000000000000888 ) ;
#2214 = DIRECTION ( 'NONE',  ( 0.000000000000000000, 0.000000000000000000, 1.000000000000000000 ) ) ;
#2215 = CIRCLE ( 'NONE', #4662, 14.54644660717763927 ) ;
#2216 = LINE ( 'NONE', #785, #17824 ) ;
#2217 = CARTESIAN_POINT ( 'NONE',  ( 3.950837973638676281, -6.316429227969383220, -13.10350451991847009 ) ) ;
#2219 = ORIENTED_EDGE ( 'NONE', *, *, #669, .F. ) ;
#2218 = LINE ( 'NONE', #7886, #4396 ) ;
#2220 = CARTESIAN_POINT ( 'NONE',  ( 2.179449471770337432, -4.500000000000000000, -3.000000000000000000 ) ) ;
#2221 = AXIS2_PLACEMENT_3D ( 'NONE', #11734, #10493, #3208 ) ;
#2222 = EDGE_LOOP ( 'NONE', ( #7269, #10524, #13507, #15791 ) ) ;
#2223 = CARTESIAN_POINT ( 'NONE',  ( 3.353306896162455697, 12.78841260990237672, 5.573563251762143622 ) ) ;
#2224 = DIRECTION ( 'NONE',  ( -0.000000000000000000, 1.000000000000000000, -0.000000000000000000 ) ) ;
#2225 = ORIENTED_EDGE ( 'NONE', *, *, #374, .F. ) ;
#2226 = EDGE_CURVE ( 'NONE', #13902, #8289, #14775, .T. ) ;
#2227 = EDGE_LOOP ( 'NONE', ( #16799, #1977, #16713, #11656 ) ) ;
#2228 = DIRECTION ( 'NONE',  ( 0.7635533937278216055, 0.5095610256143827677, 0.3966532189476653092 ) ) ;
#2229 = CARTESIAN_POINT ( 'NONE',  ( 1.321128355694181398E-14, -7.013167318348350499, 25.01316734529530095 ) ) ;
#2230 = ORIENTED_EDGE ( 'NONE', *, *, #8585, .T. ) ;
#2231 = CARTESIAN_POINT ( 'NONE',  ( 15.00000000000000711, -19.99999999999999645, 3.000000000000000000 ) ) ;
#2232 = DIRECTION ( 'NONE',  ( -0.000000000000000000, -0.000000000000000000, 1.000000000000000000 ) ) ;
#2233 = CARTESIAN_POINT ( 'NONE',  ( 1.560000000000000053, 0.8660254037844389297, -1.500000000000000000 ) ) ;
#2234 = DIRECTION ( 'NONE',  ( -1.000000000000000000, 0.000000000000000000, 0.000000000000000000 ) ) ;
#2235 = B_SPLINE_CURVE_WITH_KNOTS ( 'NONE', 3,
 ( #9726, #16810, #8125, #16724, #15460, #850 ),
 .UNSPECIFIED., .F., .F.,
 ( 4, 2, 4 ),
 ( 4.072016404827931570E-17, 0.0002014099069817292182, 0.0004028198139634177246 ),
 .UNSPECIFIED. ) ;
#2236 = SURFACE_STYLE_FILL_AREA ( #9686 ) ;
#2237 = CARTESIAN_POINT ( 'NONE',  ( 16.57210152137263393, -0.01214401161737523396, 0.008007331252332839863 ) ) ;
#2238 = DIRECTION ( 'NONE',  ( 0.000000000000000000, 0.000000000000000000, 1.000000000000000000 ) ) ;
#2239 = CARTESIAN_POINT ( 'NONE',  ( 1.846524061778019199, 7.597197846158221246, -9.853584647934303220 ) ) ;
#2240 = DIRECTION ( 'NONE',  ( -0.7561779333270775005, -0.6106991889125072959, 0.2350349629540161855 ) ) ;
#2241 = DIRECTION ( 'NONE',  ( 0.000000000000000000, 0.000000000000000000, 1.000000000000000000 ) ) ;
#2242 = SURFACE_SIDE_STYLE ('',( #3680 ) ) ;
#2243 = ORIENTED_EDGE ( 'NONE', *, *, #16628, .F. ) ;
#2244 = EDGE_CURVE ( 'NONE', #18846, #1377, #4850, .T. ) ;
#2245 = AXIS2_PLACEMENT_3D ( 'NONE', #18631, #18546, #11384 ) ;
#2246 = ADVANCED_FACE ( 'NONE', ( #13535 ), #7726, .T. ) ;
#2247 = VECTOR ( 'NONE', #6907, 1000.000000000000114 ) ;
#2248 = EDGE_CURVE ( 'NONE', #17773, #4406, #6700, .T. ) ;
#2249 = ORIENTED_EDGE ( 'NONE', *, *, #2491, .T. ) ;
#2250 = ORIENTED_EDGE ( 'NONE', *, *, #5310, .F. ) ;
#2251 = ORIENTED_EDGE ( 'NONE', *, *, #6070, .T. ) ;
#2252 = CARTESIAN_POINT ( 'NONE',  ( 1.918918678667045130, -9.738328798462433156, 7.860057224348805605 ) ) ;
#2253 = CARTESIAN_POINT ( 'NONE',  ( -1.088636994872529185, -7.500000000000003553, -14.58255216580684888 ) ) ;
#2254 = ORIENTED_EDGE ( 'NONE', *, *, #16024, .F. ) ;
#2255 = CARTESIAN_POINT ( 'NONE',  ( 16.57778382496167424, -0.01092721432669101385, 0.01018821665058845458 ) ) ;
#2256 = CARTESIAN_POINT ( 'NONE',  ( 1.847168016377982669, -11.77471791462001782, 4.022276579849913603 ) ) ;
#2257 = CARTESIAN_POINT ( 'NONE',  ( 1.342453679581834924, -3.649820028552833051, 14.34050741580205823 ) ) ;
#2258 = CARTESIAN_POINT ( 'NONE',  ( 16.56872352241294521, -0.01027347319884365333, -0.001821578298043897851 ) ) ;
#2259 = CIRCLE ( 'NONE', #11127, 2.055000000000000160 ) ;
#2260 = DIRECTION ( 'NONE',  ( -0.7561779333270775005, -0.03481510524964337439, -0.6534392409364823129 ) ) ;
#2261 = AXIS2_PLACEMENT_3D ( 'NONE', #9546, #12421, #9369 ) ;
#2262 = DIRECTION ( 'NONE',  ( -0.000000000000000000, -0.000000000000000000, -1.000000000000000000 ) ) ;
#2263 = CARTESIAN_POINT ( 'NONE',  ( 3.074695600507255655, -6.754521329824886955, 14.01296402267885988 ) ) ;
#2264 = EDGE_LOOP ( 'NONE', ( #18575, #7025, #6329, #18141 ) ) ;
#2265 = ORIENTED_EDGE ( 'NONE', *, *, #8107, .F. ) ;
#2266 = ORIENTED_EDGE ( 'NONE', *, *, #2226, .T. ) ;
#2267 = ORIENTED_EDGE ( 'NONE', *, *, #14797, .T. ) ;
#2268 = DIRECTION ( 'NONE',  ( -1.000000000000000000, -0.000000000000000000, -0.000000000000000000 ) ) ;
#2269 = DIRECTION ( 'NONE',  ( 1.540743955509788340E-33, 1.000000000000000000, 2.533398541561209262E-17 ) ) ;
#2270 = EDGE_CURVE ( 'NONE', #9430, #14370, #1591, .T. ) ;
#2271 = CARTESIAN_POINT ( 'NONE',  ( 16.56753206892534891, 0.006669401563384923064, -0.006760771273036194837 ) ) ;
#2272 = CARTESIAN_POINT ( 'NONE',  ( 16.56679352167444819, 0.009170718284672540327, 0.001518074900130682347 ) ) ;
#2273 = PLANE ( 'NONE',  #9044 ) ;
#2274 = ORIENTED_EDGE ( 'NONE', *, *, #18088, .T. ) ;
#2275 = LINE ( 'NONE', #18152, #119 ) ;
#2276 = CARTESIAN_POINT ( 'NONE',  ( -3.329573251201238815, 7.500000000000000888, -13.21489263293670113 ) ) ;
#2277 = DIRECTION ( 'NONE',  ( 2.891205793294679312E-16, -1.000000000000000000, 0.000000000000000000 ) ) ;
#2278 = CARTESIAN_POINT ( 'NONE',  ( 0.3132635586635981184, -8.495712071659319520, -10.79541209008113256 ) ) ;
#2279 = DIRECTION ( 'NONE',  ( -1.000000000000000000, -0.000000000000000000, -0.000000000000000000 ) ) ;
#2280 = CARTESIAN_POINT ( 'NONE',  ( -55.93192566395838128, 9.999999999999973355, 6.000000000000000000 ) ) ;
#2281 = B_SPLINE_CURVE_WITH_KNOTS ( 'NONE', 3,
 ( #5850, #17521, #4430, #18764, #1653, #16186 ),
 .UNSPECIFIED., .F., .F.,
 ( 4, 2, 4 ),
 ( 1.748223473168675632E-18, 0.0002017457492448088553, 0.0004034914984896159759 ),
 .UNSPECIFIED. ) ;
#2282 = CARTESIAN_POINT ( 'NONE',  ( 2.636624412717140764, -2.862162146982851763, -15.80357026013259514 ) ) ;
#2283 = AXIS2_PLACEMENT_3D ( 'NONE', #65, #14490, #17085 ) ;
#2284 = ORIENTED_EDGE ( 'NONE', *, *, #5157, .T. ) ;
#2285 = AXIS2_PLACEMENT_3D ( 'NONE', #15810, #3878, #15712 ) ;
#2287 = VERTEX_POINT ( 'NONE', #16321 ) ;
#2286 = LINE ( 'NONE', #16550, #9676 ) ;
#2288 = CARTESIAN_POINT ( 'NONE',  ( 16.56782317627811096, -0.0003415813796015412622, -0.009814734722106366327 ) ) ;
#2289 = AXIS2_PLACEMENT_3D ( 'NONE', #8684, #8591, #14413 ) ;
#2290 = EDGE_CURVE ( 'NONE', #6145, #8886, #14680, .T. ) ;
#2291 = CARTESIAN_POINT ( 'NONE',  ( 1.846138399168762101, -0.4167076046096411246, 12.43476674860266407 ) ) ;
#2292 = EDGE_LOOP ( 'NONE', ( #17599, #5760, #5139, #1468 ) ) ;
#2293 = CARTESIAN_POINT ( 'NONE',  ( -194.9999999999999716, -5.000000000000024869, 6.000000000000000000 ) ) ;
#2294 = EDGE_CURVE ( 'NONE', #12560, #15587, #14969, .T. ) ;
#2295 = CARTESIAN_POINT ( 'NONE',  ( -3.338474662713250662, -7.500000000000000888, -16.12819240262148668 ) ) ;
#2296 = VERTEX_POINT ( 'NONE', #13247 ) ;
#2297 = DIRECTION ( 'NONE',  ( 0.000000000000000000, 0.000000000000000000, 1.000000000000000000 ) ) ;
#2298 = CYLINDRICAL_SURFACE ( 'NONE', #3949, 2.499999999999992006 ) ;
#2299 =( REPRESENTATION_RELATIONSHIP ('NONE','NONE', #5200, #4478 ) REPRESENTATION_RELATIONSHIP_WITH_TRANSFORMATION ( #4239 )SHAPE_REPRESENTATION_RELATIONSHIP( ) );
#2300 = CIRCLE ( 'NONE', #14190, 3.499999999999992895 ) ;
#2301 = CARTESIAN_POINT ( 'NONE',  ( 2.636624412714236865, 0.000000000000000000, 0.000000000000000000 ) ) ;
#2302 = AXIS2_PLACEMENT_3D ( 'NONE', #14884, #14687, #4470 ) ;
#2303 = DIRECTION ( 'NONE',  ( 0.000000000000000000, 0.8660254037844384856, 0.5000000000000004441 ) ) ;
#2304 = ADVANCED_FACE ( 'NONE', ( #6184 ), #17755, .F. ) ;
#2305 = CARTESIAN_POINT ( 'NONE',  ( 0.8740779401510752056, 3.609949156401575543, -13.83508928787453662 ) ) ;
#2306 = B_SPLINE_CURVE_WITH_KNOTS ( 'NONE', 3,
 ( #6875, #12698, #14230, #5517, #18258, #15380 ),
 .UNSPECIFIED., .F., .F.,
 ( 4, 2, 4 ),
 ( 1.748223473168675632E-18, 0.0002017457492448083403, 0.0004034914984896149459 ),
 .UNSPECIFIED. ) ;
#2307 = FACE_OUTER_BOUND ( 'NONE', #16486, .T. ) ;
#2309 = ORIENTED_EDGE ( 'NONE', *, *, #74, .F. ) ;
#2308 = DIRECTION ( 'NONE',  ( -1.000000000000000000, 0.000000000000000000, 0.000000000000000000 ) ) ;
#2310 = CARTESIAN_POINT ( 'NONE',  ( 2.320521194584331148, 11.60169518685982304, -10.64885423995325198 ) ) ;
#2311 = AXIS2_PLACEMENT_3D ( 'NONE', #17021, #3920, #11247 ) ;
#2312 = ORIENTED_EDGE ( 'NONE', *, *, #7348, .T. ) ;
#2313 = CARTESIAN_POINT ( 'NONE',  ( 2.697797270744668463, 12.33058466479268844, 4.970631985779629503 ) ) ;
#2314 = CARTESIAN_POINT ( 'NONE',  ( 0.3151926232592538457, -4.318679262939536301, -13.04305446098360122 ) ) ;
#2315 = VERTEX_POINT ( 'NONE', #452 ) ;
#2316 = VERTEX_POINT ( 'NONE', #16125 ) ;
#2317 = CARTESIAN_POINT ( 'NONE',  ( 2.002547531651519996, -9.778737580845755062, 7.942910686618138705 ) ) ;
#2318 = DIRECTION ( 'NONE',  ( -1.000000000000000000, 0.000000000000000000, 0.000000000000000000 ) ) ;
#2319 = VERTEX_POINT ( 'NONE', #3201 ) ;
#2320 = CARTESIAN_POINT ( 'NONE',  ( 16.56872352241294521, -0.007512283835804365630, 0.007240717549633862542 ) ) ;
#2321 = FILL_AREA_STYLE ('',( #17216 ) ) ;
#2322 = CARTESIAN_POINT ( 'NONE',  ( 1.846955891736119071, -10.21904526726841311, -7.098901504650468652 ) ) ;
#2323 = DIRECTION ( 'NONE',  ( -0.000000000000000000, -0.000000000000000000, 1.000000000000000000 ) ) ;
#2324 = CARTESIAN_POINT ( 'NONE',  ( 0.3307726912345200776, -7.596084275798974161, 11.46720933246395369 ) ) ;
#2325 = EDGE_CURVE ( 'NONE', #5848, #17372, #4463, .T. ) ;
#2326 = AXIS2_PLACEMENT_3D ( 'NONE', #16421, #13245, #6285 ) ;
#2327 =( NAMED_UNIT ( * ) PLANE_ANGLE_UNIT ( ) SI_UNIT ( $, .RADIAN. ) );
#2328 = APPLICATION_PROTOCOL_DEFINITION ( 'draft international standard', 'automotive_design', 1998, #17423 ) ;
#2329 =( GEOMETRIC_REPRESENTATION_CONTEXT ( 3 ) GLOBAL_UNCERTAINTY_ASSIGNED_CONTEXT ( ( #207 ) ) GLOBAL_UNIT_ASSIGNED_CONTEXT ( ( #5383, #4140, #9959 ) ) REPRESENTATION_CONTEXT ( 'NONE', 'WORKASPACE' ) );
#2330 = SURFACE_STYLE_USAGE ( .BOTH. , #2593 ) ;
#2331 = DIRECTION ( 'NONE',  ( 0.000000000000000000, 0.000000000000000000, 1.000000000000000000 ) ) ;
#2332 = EDGE_CURVE ( 'NONE', #15040, #13838, #14791, .T. ) ;
#2333 = CARTESIAN_POINT ( 'NONE',  ( -117.4764150448347806, -82.42962774651277869, -88.05530248339326249 ) ) ;
#2334 = CARTESIAN_POINT ( 'NONE',  ( 22.30499999999999972, 0.000000000000000000, 0.000000000000000000 ) ) ;
#2335 = CARTESIAN_POINT ( 'NONE',  ( -30.00000000000000355, -12.50000000000000178, 3.000000000000000000 ) ) ;
#2336 = CARTESIAN_POINT ( 'NONE',  ( 0.8740779401510443414, -12.04241618260075164, -7.708543377337893077 ) ) ;
#2337 = VERTEX_POINT ( 'NONE', #5989 ) ;
#2338 = VECTOR ( 'NONE', #16459, 1000.000000000000227 ) ;
#2339 = VERTEX_POINT ( 'NONE', #10387 ) ;
#2340 = VERTEX_POINT ( 'NONE', #10291 ) ;
#2341 = ORIENTED_EDGE ( 'NONE', *, *, #6570, .F. ) ;
#2342 = VECTOR ( 'NONE', #15238, 999.9999999999998863 ) ;
#2343 = CARTESIAN_POINT ( 'NONE',  ( 0.3307726912345200776, 12.88561780039865745, -4.812300915532842005 ) ) ;
#2344 = CARTESIAN_POINT ( 'NONE',  ( 16.56822296793089322, 0.009847136207496274760, 0.002414375228568293487 ) ) ;
#2345 = CIRCLE ( 'NONE', #13023, 14.54644660717763927 ) ;
#2346 = SPHERICAL_SURFACE ( 'NONE', #2596, 5.000000000000000000 ) ;
#2347 = CIRCLE ( 'NONE', #17294, 4.750000000000000000 ) ;
#2348 = EDGE_CURVE ( 'NONE', #13773, #17548, #15125, .T. ) ;
#2349 = CIRCLE ( 'NONE', #17297, 5.000000000000000000 ) ;
#2350 = CARTESIAN_POINT ( 'NONE',  ( 2.320520222537280741, -6.542539914240626864, 14.32454429810376162 ) ) ;
#2351 = EDGE_CURVE ( 'NONE', #5784, #12010, #263, .T. ) ;
#2352 = CARTESIAN_POINT ( 'NONE',  ( 0.4754618798421162973, -10.80499583390506224, -8.775436892861234739 ) ) ;
#2353 = EDGE_CURVE ( 'NONE', #5495, #10362, #16219, .T. ) ;
#2354 = LINE ( 'NONE', #3785, #9093 ) ;
#2355 = CARTESIAN_POINT ( 'NONE',  ( 3.950837973638675393, -13.10350451991835818, -6.316429227969608817 ) ) ;
#2356 = DIRECTION ( 'NONE',  ( -1.000000000000000000, 0.000000000000000000, 0.000000000000000000 ) ) ;
#2357 = ORIENTED_EDGE ( 'NONE', *, *, #13154, .T. ) ;
#2358 = ORIENTED_EDGE ( 'NONE', *, *, #18781, .F. ) ;
#2359 = ORIENTED_EDGE ( 'NONE', *, *, #9146, .T. ) ;
#2360 = ORIENTED_EDGE ( 'NONE', *, *, #8599, .T. ) ;
#2361 = ADVANCED_FACE ( 'NONE', ( #6089 ), #7047, .F. ) ;
#2362 = CARTESIAN_POINT ( 'NONE',  ( 2.353870697619111496, -0.7635393531607235218, 12.92712089195302561 ) ) ;
#2363 = CARTESIAN_POINT ( 'NONE',  ( 2.697797270744668463, -12.33058466479264936, -4.970631985779717432 ) ) ;
#2364 = LINE ( 'NONE', #6493, #12802 ) ;
#2365 = CARTESIAN_POINT ( 'NONE',  ( -194.9999999999999716, -15.00000000000002665, -153.7432847437423789 ) ) ;
#2366 = ORIENTED_EDGE ( 'NONE', *, *, #3270, .T. ) ;
#2367 = CARTESIAN_POINT ( 'NONE',  ( 16.56822296793089322, 0.0007467251401297140970, 0.01011126603341077831 ) ) ;
#2368 = CARTESIAN_POINT ( 'NONE',  ( -194.9999999999999716, 9.999999999999976907, -2.000000000000000000 ) ) ;
#2369 = CARTESIAN_POINT ( 'NONE',  ( -0.4158217634471630397, 7.499999999999999112, -14.24727159067854387 ) ) ;
#2370 = CARTESIAN_POINT ( 'NONE',  ( 1.959212340397945562, -6.829000156128106624, -10.53510106265289359 ) ) ;
#2371 = AXIS2_PLACEMENT_3D ( 'NONE', #17344, #17739, #11904 ) ;
#2372 = CARTESIAN_POINT ( 'NONE',  ( 0.3058872367615230181, 3.664492643742949252, -13.24582953854921463 ) ) ;
#2373 = CARTESIAN_POINT ( 'NONE',  ( 3.074695600508759785, 15.30693405987895694, 2.772091048737280072 ) ) ;
#2374 = CARTESIAN_POINT ( 'NONE',  ( 3.950837973638675393, -14.31366178983251380, -2.591948120961955926 ) ) ;
#2375 = CARTESIAN_POINT ( 'NONE',  ( 1.562796894703937678, 1.635200584729765362E-15, 12.15840553252917289 ) ) ;
#2376 = ORIENTED_EDGE ( 'NONE', *, *, #1659, .T. ) ;
#2377 = EDGE_CURVE ( 'NONE', #3494, #13344, #6463, .T. ) ;
#2379 = ORIENTED_EDGE ( 'NONE', *, *, #351, .T. ) ;
#2378 = DIRECTION ( 'NONE',  ( 0.000000000000000000, 0.000000000000000000, 1.000000000000000000 ) ) ;
#2380 = CARTESIAN_POINT ( 'NONE',  ( -5.000000000000000888, 17.00000000000000000, 8.000000000000000000 ) ) ;
#2381 = LINE ( 'NONE', #18432, #8014 ) ;
#2382 = EDGE_CURVE ( 'NONE', #13257, #7625, #18395, .T. ) ;
#2383 = ORIENTED_EDGE ( 'NONE', *, *, #18035, .F. ) ;
#2384 = LINE ( 'NONE', #15566, #10687 ) ;
#2385 = DIRECTION ( 'NONE',  ( -1.000000000000000000, 0.000000000000000000, 0.000000000000000000 ) ) ;
#2386 = ORIENTED_EDGE ( 'NONE', *, *, #1455, .T. ) ;
#2387 = LINE ( 'NONE', #15298, #17614 ) ;
#2388 = CARTESIAN_POINT ( 'NONE',  ( -199.9999999999999716, -30.00000000000003197, 3.000000000000000000 ) ) ;
#2389 = DIRECTION ( 'NONE',  ( -0.000000000000000000, -0.000000000000000000, 1.000000000000000000 ) ) ;
#2390 = FACE_OUTER_BOUND ( 'NONE', #11983, .T. ) ;
#2391 = DIRECTION ( 'NONE',  ( 1.000000000000000000, 0.000000000000000000, 0.000000000000000000 ) ) ;
#2392 = ADVANCED_FACE ( 'NONE', ( #6383 ), #8279, .T. ) ;
#2393 = CARTESIAN_POINT ( 'NONE',  ( 3.377929128793399016, 10.50432311212916225, -9.234024516648208447 ) ) ;
#2395 = ORIENTED_EDGE ( 'NONE', *, *, #9782, .F. ) ;
#2394 = CARTESIAN_POINT ( 'NONE',  ( -61.35602477868047799, -15.00000000000000711, 6.000000000000000000 ) ) ;
#2396 = CARTESIAN_POINT ( 'NONE',  ( 0.4385251269669950824, 0.7363879510387324467, -13.84299131624728751 ) ) ;
#2397 =( BOUNDED_SURFACE ( )  B_SPLINE_SURFACE ( 3, 1, ( 
 ( #17527, #4435 ),
 ( #18509, #5859 ),
 ( #14112, #8209 ),
 ( #11699, #13225 ) ),
 .UNSPECIFIED., .F., .F., .T. ) 
 B_SPLINE_SURFACE_WITH_KNOTS ( ( 4, 4 ),
 ( 2, 2 ),
 ( 0.000000000000000000, 1.000000000000000000 ),
 ( 0.000000000000000000, 1.000000000000000000 ),
 .UNSPECIFIED. ) 
 GEOMETRIC_REPRESENTATION_ITEM ( )  RATIONAL_B_SPLINE_SURFACE ( (
 ( 1.000000000000000000, 1.000000000000000000),
 ( 0.7792777138730158093, 0.9689936506012928330),
 ( 0.7792777138730158093, 0.9689936506012928330),
 ( 1.000000000000000000, 1.000000000000000000) ) ) 
 REPRESENTATION_ITEM ( '' )  SURFACE ( )  );
#2398 = CARTESIAN_POINT ( 'NONE',  ( 0.3137051932979757485, -11.37800749014125223, -7.698472063774596030 ) ) ;
#2399 = CARTESIAN_POINT ( 'NONE',  ( 1.918921323896324083, 4.466082741316370175, -11.69058285425785648 ) ) ;
#2400 = EDGE_CURVE ( 'NONE', #5315, #2529, #4631, .T. ) ;
#2401 = ORIENTED_EDGE ( 'NONE', *, *, #9051, .T. ) ;
#2402 = ORIENTED_EDGE ( 'NONE', *, *, #14786, .F. ) ;
#2403 = LINE ( 'NONE', #3749, #1092 ) ;
#2404 = CYLINDRICAL_SURFACE ( 'NONE', #17854, 2.750000000000000000 ) ;
#2405 = ORIENTED_EDGE ( 'NONE', *, *, #11806, .T. ) ;
#2406 = CARTESIAN_POINT ( 'NONE',  ( 1.845756295923363099, -0.4783934145701149721, -12.43231724724606835 ) ) ;
#2407 = EDGE_CURVE ( 'NONE', #9019, #11032, #3599, .T. ) ;
#2408 = CARTESIAN_POINT ( 'NONE',  ( 2.002547531651519996, -11.75462648437105173, 4.532360870844282630 ) ) ;
#2409 = SURFACE_STYLE_FILL_AREA ( #3573 ) ;
#2410 = AXIS2_PLACEMENT_3D ( 'NONE', #3830, #2035, #12340 ) ;
#2411 = CARTESIAN_POINT ( 'NONE',  ( 1.845755665166725068, 12.43231320373361193, 0.4784952423728983106 ) ) ;
#2413 = DIRECTION ( 'NONE',  ( -1.000000000000000000, -0.000000000000000000, -0.000000000000000000 ) ) ;
#2412 = AXIS2_PLACEMENT_3D ( 'NONE', #1147, #1042, #8054 ) ;
#2414 = CARTESIAN_POINT ( 'NONE',  ( 2.002547531651519996, 0.6781519942173496185, -12.57989064830758785 ) ) ;
#2415 = APPLICATION_PROTOCOL_DEFINITION ( 'draft international standard', 'automotive_design', 1998, #13520 ) ;
#2416 = SHAPE_REPRESENTATION_RELATIONSHIP ( 'NONE' , 'NONE' ,  #14858, #5341 ) ;
#2417 = CYLINDRICAL_SURFACE ( 'NONE', #2513, 4.999999999999997335 ) ;
#2418 = FACE_OUTER_BOUND ( 'NONE', #2292, .T. ) ;
#2419 = CARTESIAN_POINT ( 'NONE',  ( 1.847412631396507576, -3.804043368582581408, -11.84727953344286888 ) ) ;
#2420 = CARTESIAN_POINT ( 'NONE',  ( 0.3720661004400040439, 13.34435358167253227, 3.575426119359231603 ) ) ;
#2421 = AXIS2_PLACEMENT_3D ( 'NONE', #9557, #5349, #6879 ) ;
#2422 = CARTESIAN_POINT ( 'NONE',  ( 0.4862570985993235340, -11.67702470553359539, -7.559321496869553236 ) ) ;
#2423 = CARTESIAN_POINT ( 'NONE',  ( 1.562796894703937678, 0.000000000000000000, 0.000000000000000000 ) ) ;
#2424 = ORIENTED_EDGE ( 'NONE', *, *, #17068, .T. ) ;
#2425 = EDGE_CURVE ( 'NONE', #4745, #12842, #13817, .T. ) ;
#2426 = ORIENTED_EDGE ( 'NONE', *, *, #3537, .F. ) ;
#2427 = VERTEX_POINT ( 'NONE', #12386 ) ;
#2428 = ORIENTED_EDGE ( 'NONE', *, *, #11183, .T. ) ;
#2429 = EDGE_CURVE ( 'NONE', #10554, #18537, #299, .T. ) ;
#2430 = CARTESIAN_POINT ( 'NONE',  ( 1.846138399168762101, -0.4167076046094680408, -12.43476674860266940 ) ) ;
#2431 = CARTESIAN_POINT ( 'NONE',  ( -2.563381608035275594, -7.500000000000003553, -15.65171369207284791 ) ) ;
#2432 = DIRECTION ( 'NONE',  ( 1.000000000000000000, 0.000000000000000000, 0.000000000000000000 ) ) ;
#2433 = CARTESIAN_POINT ( 'NONE',  ( 16.56753206892534891, 0.009389754735542247058, 0.001421777558675981282 ) ) ;
#2434 = DIRECTION ( 'NONE',  ( -0.7635533937278214944, 0.5095610256143914274, -0.3966532189476541514 ) ) ;
#2435 = CARTESIAN_POINT ( 'NONE',  ( 0.3095370825347233956, -12.91933430393611104, 4.681152801286112997 ) ) ;
#2436 = LINE ( 'NONE', #5579, #11204 ) ;
#2437 = ORIENTED_EDGE ( 'NONE', *, *, #12827, .F. ) ;
#2438 = EDGE_LOOP ( 'NONE', ( #5584, #5199, #7981, #10841 ) ) ;
#2439 = VERTEX_POINT ( 'NONE', #18580 ) ;
#2440 = ORIENTED_EDGE ( 'NONE', *, *, #14630, .T. ) ;
#2441 = ADVANCED_FACE ( 'NONE', ( #15615 ), #1280, .F. ) ;
#2442 = EDGE_CURVE ( 'NONE', #5851, #5315, #17628, .T. ) ;
#2443 = EDGE_CURVE ( 'NONE', #11616, #6154, #11463, .T. ) ;
#2444 = CARTESIAN_POINT ( 'NONE',  ( -5.000000000000000000, 6.123233995736766282E-16, -3.000000000000000000 ) ) ;
#2445 = CARTESIAN_POINT ( 'NONE',  ( 0.3720661004400037664, 7.524064345033464107, 11.58636699658217672 ) ) ;
#2446 = CARTESIAN_POINT ( 'NONE',  ( 0.4754618798421167414, -11.68486377711971613, 7.564402563418431313 ) ) ;
#2447 = FACE_OUTER_BOUND ( 'NONE', #4107, .T. ) ;
#2448 =( LENGTH_UNIT ( ) NAMED_UNIT ( * ) SI_UNIT ( .MILLI., .METRE. ) );
#2449 = ORIENTED_EDGE ( 'NONE', *, *, #15428, .T. ) ;
#2450 = CARTESIAN_POINT ( 'NONE',  ( 6.231098469233193882, 7.500000000000000000, -17.00000000000000000 ) ) ;
#2451 = CARTESIAN_POINT ( 'NONE',  ( 5.616333669597326050, 4.188188789804502044, -12.00000000261158917 ) ) ;
#2452 = CARTESIAN_POINT ( 'NONE',  ( 1.560000000000000053, -1.732050807568877859, -1.752539433813135784E-17 ) ) ;
#2453 = CARTESIAN_POINT ( 'NONE',  ( 2.636624412715137922, -15.91454522070252153, 2.161493821597598508 ) ) ;
#2454 = CARTESIAN_POINT ( 'NONE',  ( 1.847247051441592625, 3.685275815977189673, 11.88474976472813971 ) ) ;
#2455 = CARTESIAN_POINT ( 'NONE',  ( 0.000000000000000000, 0.000000000000000000, -12.00000000000000000 ) ) ;
#2456 = ORIENTED_EDGE ( 'NONE', *, *, #6278, .T. ) ;
#2458 = ORIENTED_EDGE ( 'NONE', *, *, #9502, .T. ) ;
#2457 = CARTESIAN_POINT ( 'NONE',  ( 0.3095370825347233956, 0.4597470195090213041, 13.73357284481724960 ) ) ;
#2459 = CARTESIAN_POINT ( 'NONE',  ( 1.342453679581834924, -13.74702459364880269, -5.476372339890162699 ) ) ;
#2460 = CIRCLE ( 'NONE', #3389, 5.000000000000004441 ) ;
#2461 = DIRECTION ( 'NONE',  ( 0.000000000000000000, 0.000000000000000000, 1.000000000000000000 ) ) ;
#2462 = ADVANCED_FACE ( 'NONE', ( #11521 ), #3966, .T. ) ;
#2463 = EDGE_CURVE ( 'NONE', #9741, #9678, #8379, .T. ) ;
#2464 = EDGE_LOOP ( 'NONE', ( #11141, #1803, #13657, #3611 ) ) ;
#2465 = EDGE_CURVE ( 'NONE', #322, #12162, #9670, .T. ) ;
#2466 = CARTESIAN_POINT ( 'NONE',  ( 1.847247051441591958, -3.685275815977108405, -11.88474976472816103 ) ) ;
#2467 = DIRECTION ( 'NONE',  ( 0.7635533937278216055, -0.2197766120036547532, 0.6071939193889553943 ) ) ;
#2468 = ADVANCED_FACE ( 'NONE', ( #1091 ), #17534, .F. ) ;
#2470 = CARTESIAN_POINT ( 'NONE',  ( 0.4754618798421162973, 13.45049478164060019, 3.583352865732715387 ) ) ;
#2469 =( BOUNDED_SURFACE ( )  B_SPLINE_SURFACE ( 3, 1, ( 
 ( #991, #11234 ),
 ( #14279, #2420 ),
 ( #5651, #16959 ),
 ( #8270, #6827 ) ),
 .UNSPECIFIED., .F., .F., .T. ) 
 B_SPLINE_SURFACE_WITH_KNOTS ( ( 4, 4 ),
 ( 2, 2 ),
 ( 0.000000000000000000, 1.000000000000000000 ),
 ( 0.000000000000000000, 1.000000000000000000 ),
 .UNSPECIFIED. ) 
 GEOMETRIC_REPRESENTATION_ITEM ( )  RATIONAL_B_SPLINE_SURFACE ( (
 ( 1.000000000000000000, 1.000000000000000000),
 ( 0.9933953342250438912, 0.8357391271907739227),
 ( 0.9933953342250438912, 0.8357391271907739227),
 ( 1.000000000000000000, 1.000000000000000000) ) ) 
 REPRESENTATION_ITEM ( '' )  SURFACE ( )  );
#2471 = ORIENTED_EDGE ( 'NONE', *, *, #4755, .T. ) ;
#2472 = CARTESIAN_POINT ( 'NONE',  ( 1.846524061778018977, -7.597197846158149304, 9.853584647934361840 ) ) ;
#2473 = LINE ( 'NONE', #5445, #8530 ) ;
#2474 = CARTESIAN_POINT ( 'NONE',  ( 0.4862570985993235340, 13.89016912371017476, 0.7479633556562934604 ) ) ;
#2475 = CYLINDRICAL_SURFACE ( 'NONE', #6597, 4.750000000000000000 ) ;
#2476 = CARTESIAN_POINT ( 'NONE',  ( 1.861706995891668770, 7.751853334747318414, 9.751699138048461890 ) ) ;
#2477 = CARTESIAN_POINT ( 'NONE',  ( 8.438534575730034959, -1.899950616255234870, 6.598402093327873530 ) ) ;
#2478 = VECTOR ( 'NONE', #4601, 1000.000000000000114 ) ;
#2479 = CARTESIAN_POINT ( 'NONE',  ( 16.56679352167444819, -0.004162264567718857756, 0.008311568981097966838 ) ) ;
#2481 = VERTEX_POINT ( 'NONE', #14291 ) ;
#2480 = CARTESIAN_POINT ( 'NONE',  ( 1.918921323896325193, 6.832782632379378107, 10.48468902844554052 ) ) ;
#2482 = CARTESIAN_POINT ( 'NONE',  ( 2.636624412717099908, 11.60464335004051861, -11.10302021258208249 ) ) ;
#2483 = CARTESIAN_POINT ( 'NONE',  ( 1.977228804422058728, -14.12033626431055211, 6.152949558601312319 ) ) ;
#2484 = CARTESIAN_POINT ( 'NONE',  ( 0.3137051932979792457, -3.805684345189695783, -13.20008686438109891 ) ) ;
#2485 = VERTEX_POINT ( 'NONE', #1192 ) ;
#2486 = LINE ( 'NONE', #15588, #1791 ) ;
#2487 = FACE_OUTER_BOUND ( 'NONE', #15895, .T. ) ;
#2488 = ORIENTED_EDGE ( 'NONE', *, *, #14493, .T. ) ;
#2489 = CARTESIAN_POINT ( 'NONE',  ( 0.3142014840576534684, 3.879477880151442015, 13.17932813834296013 ) ) ;
#2490 = CARTESIAN_POINT ( 'NONE',  ( 0.000000000000000000, 1.732050807568878747, 7.017607234860990640E-28 ) ) ;
#2491 = EDGE_CURVE ( 'NONE', #2548, #14769, #13939, .T. ) ;
#2492 = CARTESIAN_POINT ( 'NONE',  ( 16.57778382496167424, -0.01018821665058785610, 0.01092721432668990016 ) ) ;
#2493 = CIRCLE ( 'NONE', #11370, 2.055000000000000160 ) ;
#2494 = CARTESIAN_POINT ( 'NONE',  ( 1.254255976357135038, 3.563435620217683120, 14.24071337840730322 ) ) ;
#2495 = CARTESIAN_POINT ( 'NONE',  ( 2.636624412717099908, 15.80357026013547816, -2.862162146981609201 ) ) ;
#2496 = UNCERTAINTY_MEASURE_WITH_UNIT (LENGTH_MEASURE( 1.000000000000000082E-05 ), #1765, 'distance_accuracy_value', 'NONE');
#2497 = SHAPE_DEFINITION_REPRESENTATION ( #4797, #12894 ) ;
#2498 = B_SPLINE_CURVE_WITH_KNOTS ( 'NONE', 3,
 ( #10543, #16653, #1944, #16566, #17904, #13400, #6345, #12345, #14832, #696, #3359, #6146, #1749 ),
 .UNSPECIFIED., .F., .F.,
 ( 4, 3, 3, 3, 4 ),
 ( 8.673617379884035472E-19, 0.0002299804304191502627, 0.0004599608082120273944, 0.0006467586077648031012, 0.0008336169836825989407 ),
 .UNSPECIFIED. ) ;
#2499 = CARTESIAN_POINT ( 'NONE',  ( 0.3058872367615230181, 7.578326039752771415, -11.46514199369349818 ) ) ;
#2500 = CARTESIAN_POINT ( 'NONE',  ( 0.3095370825347234511, -12.91933430393604532, -4.681152801286298626 ) ) ;
#2501 =( BOUNDED_SURFACE ( )  B_SPLINE_SURFACE ( 3, 1, ( 
 ( #2091, #13649 ),
 ( #12302, #5033 ),
 ( #15440, #2257 ),
 ( #9345, #18227 ) ),
 .UNSPECIFIED., .F., .F., .T. ) 
 B_SPLINE_SURFACE_WITH_KNOTS ( ( 4, 4 ),
 ( 2, 2 ),
 ( 0.000000000000000000, 1.000000000000000000 ),
 ( 0.000000000000000000, 1.000000000000000000 ),
 .UNSPECIFIED. ) 
 GEOMETRIC_REPRESENTATION_ITEM ( )  RATIONAL_B_SPLINE_SURFACE ( (
 ( 1.000000000000000000, 1.000000000000000000),
 ( 0.7792777138730158093, 0.9689936506012928330),
 ( 0.7792777138730158093, 0.9689936506012928330),
 ( 1.000000000000000000, 1.000000000000000000) ) ) 
 REPRESENTATION_ITEM ( '' )  SURFACE ( )  );
#2502 =( BOUNDED_SURFACE ( )  B_SPLINE_SURFACE ( 3, 1, ( 
 ( #16630, #4591 ),
 ( #14807, #10413 ),
 ( #12240, #7951 ),
 ( #13757, #10709 ) ),
 .UNSPECIFIED., .F., .F., .T. ) 
 B_SPLINE_SURFACE_WITH_KNOTS ( ( 4, 4 ),
 ( 2, 2 ),
 ( 0.000000000000000000, 1.000000000000000000 ),
 ( 0.000000000000000000, 1.000000000000000000 ),
 .UNSPECIFIED. ) 
 GEOMETRIC_REPRESENTATION_ITEM ( )  RATIONAL_B_SPLINE_SURFACE ( (
 ( 1.000000000000000000, 1.000000000000000000),
 ( 0.9933953342250438912, 0.8357391271907739227),
 ( 0.9933953342250438912, 0.8357391271907739227),
 ( 1.000000000000000000, 1.000000000000000000) ) ) 
 REPRESENTATION_ITEM ( '' )  SURFACE ( )  );
#2503 = CARTESIAN_POINT ( 'NONE',  ( 0.3137051932979757485, -4.679953077377398074, -12.91601973349275134 ) ) ;
#2504 = DIRECTION ( 'NONE',  ( -1.000000000000000000, 0.000000000000000000, 0.000000000000000000 ) ) ;
#2505 = EDGE_CURVE ( 'NONE', #14390, #5155, #11303, .T. ) ;
#2506 = CARTESIAN_POINT ( 'NONE',  ( 1.560000000000000053, -0.8660254037844384856, 1.500000000000000000 ) ) ;
#2507 = VERTEX_POINT ( 'NONE', #7414 ) ;
#2508 = ORIENTED_EDGE ( 'NONE', *, *, #4966, .F. ) ;
#2509 = ORIENTED_EDGE ( 'NONE', *, *, #7144, .T. ) ;
#2510 = EDGE_CURVE ( 'NONE', #287, #15231, #12446, .T. ) ;
#2511 = ORIENTED_EDGE ( 'NONE', *, *, #3757, .T. ) ;
#2512 = EDGE_CURVE ( 'NONE', #885, #14287, #15861, .T. ) ;
#2513 = AXIS2_PLACEMENT_3D ( 'NONE', #6741, #8534, #5291 ) ;
#2514 = CARTESIAN_POINT ( 'NONE',  ( 8.522092701127531811, 5.397361180353144050, 4.388629235579598387 ) ) ;
#2515 = DIRECTION ( 'NONE',  ( 0.000000000000000000, 0.000000000000000000, -1.000000000000000000 ) ) ;
#2516 = DIRECTION ( 'NONE',  ( 1.000000000000000000, 0.000000000000000000, 0.000000000000000000 ) ) ;
#2517 = DIRECTION ( 'NONE',  ( -0.7561779333270775005, 0.6534392409364818688, -0.03481510524965020920 ) ) ;
#2518 = DIRECTION ( 'NONE',  ( 1.000000000000000000, 0.000000000000000000, 2.775557561562889773E-15 ) ) ;
#2519 = DIRECTION ( 'NONE',  ( -1.000000000000000000, 0.000000000000000000, 0.000000000000000000 ) ) ;
#2520 = CARTESIAN_POINT ( 'NONE',  ( 0.000000000000000000, 0.000000000000000000, 10.49999999999999822 ) ) ;
#2521 = CARTESIAN_POINT ( 'NONE',  ( 2.123976203522053297, 1.531817366691969884, -15.54801196254785189 ) ) ;
#2522 = CARTESIAN_POINT ( 'NONE',  ( -7.000000000000000000, 0.000000000000000000, 8.000000000000000000 ) ) ;
#2523 = AXIS2_PLACEMENT_3D ( 'NONE', #14864, #2992, #16408 ) ;
#2524 = EDGE_CURVE ( 'NONE', #11551, #1902, #9126, .T. ) ;
#2525 = ORIENTED_EDGE ( 'NONE', *, *, #9512, .F. ) ;
#2526 = B_SPLINE_CURVE_WITH_KNOTS ( 'NONE', 3,
 ( #5948, #7788, #703, #419, #18097, #6247 ),
 .UNSPECIFIED., .F., .F.,
 ( 4, 2, 4 ),
 ( 0.000000000000000000, 0.001656992708823057468, 0.003313985417646114935 ),
 .UNSPECIFIED. ) ;
#2527 = ORIENTED_EDGE ( 'NONE', *, *, #744, .F. ) ;
#2528 = EDGE_CURVE ( 'NONE', #7625, #15007, #18216, .T. ) ;
#2529 = VERTEX_POINT ( 'NONE', #17634 ) ;
#2530 = ORIENTED_EDGE ( 'NONE', *, *, #14186, .T. ) ;
#2531 = DIRECTION ( 'NONE',  ( 0.000000000000000000, 0.000000000000000000, 1.000000000000000000 ) ) ;
#2532 = DIRECTION ( 'NONE',  ( 0.000000000000000000, -0.2588190451025214611, -0.9659258262890679791 ) ) ;
#2533 = CARTESIAN_POINT ( 'NONE',  ( 0.3095370825347234511, 13.73357284481724783, 0.4597470195090685441 ) ) ;
#2534 = CARTESIAN_POINT ( 'NONE',  ( -30.00000000000000355, -12.50000000000000178, -0.5000000000000000000 ) ) ;
#2535 = ORIENTED_EDGE ( 'NONE', *, *, #14122, .T. ) ;
#2536 = CARTESIAN_POINT ( 'NONE',  ( 0.3058872367615226295, 8.562166468153870724, -10.75034008168906396 ) ) ;
#2537 = CARTESIAN_POINT ( 'NONE',  ( 1.918921323896324083, -12.08297777410667173, 3.258415356426475729 ) ) ;
#2538 = AXIS2_PLACEMENT_3D ( 'NONE', #7054, #5593, #17264 ) ;
#2539 = CARTESIAN_POINT ( 'NONE',  ( 6.009712068683786157, 3.596569907853440551, -12.00000000129651312 ) ) ;
#2540 = CARTESIAN_POINT ( 'NONE',  ( 1.846138399168762101, -6.971848976710933954, -10.30487220521577818 ) ) ;
#2541 = PRODUCT_DEFINITION_FORMATION_WITH_SPECIFIED_SOURCE ( 'ANY', '', #12278, .NOT_KNOWN. ) ;
#2542 = CARTESIAN_POINT ( 'NONE',  ( 1.254009781011253821, 14.24044713813288254, 3.563484327698356324 ) ) ;
#2543 = CARTESIAN_POINT ( 'NONE',  ( 1.846138399168762989, 4.238866729160403857, 11.69739621335923729 ) ) ;
#2544 = CARTESIAN_POINT ( 'NONE',  ( 0.3307726912345222980, 4.812300915532974344, 12.88561780039860416 ) ) ;
#2545 = B_SPLINE_CURVE_WITH_KNOTS ( 'NONE', 3,
 ( #15786, #14352, #4232, #1258, #7096, #15880 ),
 .UNSPECIFIED., .F., .F.,
 ( 4, 2, 4 ),
 ( 3.144186300207962859E-18, 0.0002017457492448088553, 0.0004034914984896145664 ),
 .UNSPECIFIED. ) ;
#2546 = CARTESIAN_POINT ( 'NONE',  ( 1.847412631396500693, -3.886120457021478902, 11.82061107079963413 ) ) ;
#2547 = EDGE_CURVE ( 'NONE', #15093, #13901, #16786, .T. ) ;
#2548 = VERTEX_POINT ( 'NONE', #5961 ) ;
#2550 = EDGE_LOOP ( 'NONE', ( #637, #18050, #16118, #16333, #10887, #17674 ) ) ;
#2549 = FACE_OUTER_BOUND ( 'NONE', #3127, .T. ) ;
#2551 = DIRECTION ( 'NONE',  ( 0.000000000000000000, 0.000000000000000000, -1.000000000000000000 ) ) ;
#2552 = CARTESIAN_POINT ( 'NONE',  ( 1.254255976357310010, 14.64488542023430817, 1.011593778944276822 ) ) ;
#2553 = ORIENTED_EDGE ( 'NONE', *, *, #12004, .F. ) ;
#2554 = DIRECTION ( 'NONE',  ( -1.000000000000000000, -0.000000000000000000, -0.000000000000000000 ) ) ;
#2555 = CARTESIAN_POINT ( 'NONE',  ( 1.847372867223026294, -12.44269075185938611, -0.1054171785007791406 ) ) ;
#2556 = CARTESIAN_POINT ( 'NONE',  ( 2.636624412714236865, 0.000000000000000000, 0.000000000000000000 ) ) ;
#2557 = DIRECTION ( 'NONE',  ( 0.000000000000000000, 1.000000000000000000, 0.000000000000000000 ) ) ;
#2558 = VERTEX_POINT ( 'NONE', #10462 ) ;
#2559 = CARTESIAN_POINT ( 'NONE',  ( 1.847461586945730261, -7.286856109515127855, 10.08650590720933771 ) ) ;
#2560 = CARTESIAN_POINT ( 'NONE',  ( 0.3132635586635978409, 13.72732610560088773, -0.5277914263193584921 ) ) ;
#2561 = CARTESIAN_POINT ( 'NONE',  ( 1.847034903785822690, 12.44051878787773191, 0.2299360331934612034 ) ) ;
#2562 = CARTESIAN_POINT ( 'NONE',  ( 0.3150686449036049219, -13.11344473514185971, -4.099563462784791668 ) ) ;
#2563 = CONICAL_SURFACE ( 'NONE', #5932, 14.54644660717763927, 0.8559913436420816257 ) ;
#2564 = DIRECTION ( 'NONE',  ( 1.000000000000000000, 0.000000000000000000, 0.000000000000000000 ) ) ;
#2565 = AXIS2_PLACEMENT_3D ( 'NONE', #15567, #14134, #2743 ) ;
#2566 = EDGE_CURVE ( 'NONE', #18408, #6600, #3875, .T. ) ;
#2567 = DIRECTION ( 'NONE',  ( 1.000000000000000000, 0.000000000000000000, 0.000000000000000000 ) ) ;
#2568 = LINE ( 'NONE', #13868, #15057 ) ;
#2569 = ADVANCED_FACE ( 'NONE', ( #3178 ), #13135, .T. ) ;
#2570 = ADVANCED_FACE ( 'NONE', ( #11802 ), #7909, .F. ) ;
#2571 = B_SPLINE_CURVE_WITH_KNOTS ( 'NONE', 3,
 ( #15859, #5810, #17197, #17482, #1527, #1144 ),
 .UNSPECIFIED., .F., .F.,
 ( 4, 2, 4 ),
 ( 0.000000000000000000, 0.0001828790815886946713, 0.0003657581631773893427 ),
 .UNSPECIFIED. ) ;
#2572 = PLANE ( 'NONE',  #2187 ) ;
#2574 = ORIENTED_EDGE ( 'NONE', *, *, #15665, .F. ) ;
#2573 = CARTESIAN_POINT ( 'NONE',  ( 2.002547531651520885, 10.57595306287292480, 6.845637710436228929 ) ) ;
#2575 = CARTESIAN_POINT ( 'NONE',  ( 16.56753206892534891, 0.009389754735542245323, 0.001421777558675984534 ) ) ;
#2576 = CARTESIAN_POINT ( 'NONE',  ( 2.636624412715137922, -7.605649742761668719, 14.14563173255331741 ) ) ;
#2577 =( BOUNDED_SURFACE ( )  B_SPLINE_SURFACE ( 3, 1, ( 
 ( #1198, #7036 ),
 ( #1291, #12853 ),
 ( #15621, #11158 ),
 ( #15535, #2435 ) ),
 .UNSPECIFIED., .F., .F., .T. ) 
 B_SPLINE_SURFACE_WITH_KNOTS ( ( 4, 4 ),
 ( 2, 2 ),
 ( 0.000000000000000000, 1.000000000000000000 ),
 ( 0.000000000000000000, 1.000000000000000000 ),
 .UNSPECIFIED. ) 
 GEOMETRIC_REPRESENTATION_ITEM ( )  RATIONAL_B_SPLINE_SURFACE ( (
 ( 1.000000000000000000, 1.000000000000000000),
 ( 0.9933953342250438912, 0.8357391271907739227),
 ( 0.9933953342250438912, 0.8357391271907739227),
 ( 1.000000000000000000, 1.000000000000000000) ) ) 
 REPRESENTATION_ITEM ( '' )  SURFACE ( )  );
#2578 = ORIENTED_EDGE ( 'NONE', *, *, #950, .T. ) ;
#2579 = CARTESIAN_POINT ( 'NONE',  ( 0.3150686449036048109, 4.099563462784836965, -13.11344473514184372 ) ) ;
#2580 = AXIS2_PLACEMENT_3D ( 'NONE', #13797, #8261, #5192 ) ;
#2581 = CARTESIAN_POINT ( 'NONE',  ( 0.8740779401510756497, -5.211551231203870316, -13.31469722824378721 ) ) ;
#2582 = VECTOR ( 'NONE', #12525, 1000.000000000000114 ) ;
#2583 = ADVANCED_BREP_SHAPE_REPRESENTATION ( '', ( #3619, #2030 ), #8722 ) ;
#2584 = ORIENTED_EDGE ( 'NONE', *, *, #17542, .F. ) ;
#2585 = CARTESIAN_POINT ( 'NONE',  ( 0.3145729642390374670, 4.535980493005085989, 12.96842777670208768 ) ) ;
#2586 = AXIS2_PLACEMENT_3D ( 'NONE', #13929, #6682, #1015 ) ;
#2587 = CARTESIAN_POINT ( 'NONE',  ( 16.58200780006414732, 0.009393638146079845430, -0.006043560077721606832 ) ) ;
#2588 = DIRECTION ( 'NONE',  ( 1.000000000000000000, -0.000000000000000000, -0.000000000000000000 ) ) ;
#2589 = CARTESIAN_POINT ( 'NONE',  ( 5.000000000000000000, 0.000000000000000000, -3.000000000000000000 ) ) ;
#2590 = CARTESIAN_POINT ( 'NONE',  ( 1.846955891736114852, -9.909315188408097441, 7.525208385419928092 ) ) ;
#2591 = ORIENTED_EDGE ( 'NONE', *, *, #12297, .F. ) ;
#2592 = CONTEXT_DEPENDENT_SHAPE_REPRESENTATION ( #15001, #17441 ) ;
#2593 = SURFACE_SIDE_STYLE ('',( #6822 ) ) ;
#2594 = DIRECTION ( 'NONE',  ( 1.000000000000000000, 0.000000000000000000, 0.000000000000000000 ) ) ;
#2595 = CARTESIAN_POINT ( 'NONE',  ( -59.99999999999997158, -10.00000000000000888, 6.000000000000000000 ) ) ;
#2596 = AXIS2_PLACEMENT_3D ( 'NONE', #13911, #2432, #17247 ) ;
#2597 = CARTESIAN_POINT ( 'NONE',  ( 1.847426409206469611, 0.06227732482722434654, 12.44303504652092762 ) ) ;
#2598 = CARTESIAN_POINT ( 'NONE',  ( 2.636624412716062071, -14.14563173255412742, -7.605649742760987486 ) ) ;
#2599 = DIRECTION ( 'NONE',  ( -0.000000000000000000, -0.000000000000000000, 1.000000000000000000 ) ) ;
#2600 = EDGE_CURVE ( 'NONE', #9475, #15162, #14038, .T. ) ;
#2601 = ORIENTED_EDGE ( 'NONE', *, *, #14232, .F. ) ;
#2602 = DIRECTION ( 'NONE',  ( 1.000000000000000000, 0.000000000000000000, 0.000000000000000000 ) ) ;
#2603 = FILL_AREA_STYLE_COLOUR ( '', #2637 ) ;
#2604 = VERTEX_POINT ( 'NONE', #13798 ) ;
#2605 = ORIENTED_EDGE ( 'NONE', *, *, #2244, .T. ) ;
#2606 = EDGE_LOOP ( 'NONE', ( #448, #11624, #6831, #11583 ) ) ;
#2607 = CARTESIAN_POINT ( 'NONE',  ( 1.562796894703937678, 0.000000000000000000, 5.000000000000000000 ) ) ;
#2608 = EDGE_LOOP ( 'NONE', ( #12969, #10556, #8475, #1564 ) ) ;
#2609 = EDGE_CURVE ( 'NONE', #4344, #11616, #13598, .T. ) ;
#2610 = AXIS2_PLACEMENT_3D ( 'NONE', #39, #18864, #1378 ) ;
#2611 = MECHANICAL_DESIGN_GEOMETRIC_PRESENTATION_REPRESENTATION (  '', ( #10889 ), #16049 ) ;
#2612 = CARTESIAN_POINT ( 'NONE',  ( 1.847426409206450959, -2.029922383240494730E-11, 12.44303504652081038 ) ) ;
#2613 = CARTESIAN_POINT ( 'NONE',  ( 0.3137051932979809665, 13.20008686438111312, -3.805684345189650042 ) ) ;
#2614 = CARTESIAN_POINT ( 'NONE',  ( 16.56782317627811096, -0.005492611183758475124, -0.008141063682853461742 ) ) ;
#2616 = FACE_OUTER_BOUND ( 'NONE', #12084, .T. ) ;
#2615 =( BOUNDED_SURFACE ( )  B_SPLINE_SURFACE ( 3, 1, ( 
 ( #9616, #17694 ),
 ( #295, #6127 ),
 ( #5670, #4265 ),
 ( #11527, #10084 ) ),
 .UNSPECIFIED., .F., .F., .T. ) 
 B_SPLINE_SURFACE_WITH_KNOTS ( ( 4, 4 ),
 ( 2, 2 ),
 ( 0.000000000000000000, 1.000000000000000000 ),
 ( 0.000000000000000000, 1.000000000000000000 ),
 .UNSPECIFIED. ) 
 GEOMETRIC_REPRESENTATION_ITEM ( )  RATIONAL_B_SPLINE_SURFACE ( (
 ( 1.000000000000000000, 1.000000000000000000),
 ( 0.9593108457356467333, 0.9995965569486454649),
 ( 0.9593108457356467333, 0.9995965569486454649),
 ( 1.000000000000000000, 1.000000000000000000) ) ) 
 REPRESENTATION_ITEM ( '' )  SURFACE ( )  );
#2617 = FACE_OUTER_BOUND ( 'NONE', #13214, .T. ) ;
#2618 = DIRECTION ( 'NONE',  ( 0.000000000000000000, 0.000000000000000000, -1.000000000000000000 ) ) ;
#2619 = EDGE_CURVE ( 'NONE', #14675, #8361, #3337, .T. ) ;
#2620 = CARTESIAN_POINT ( 'NONE',  ( 16.57778382496167424, 0.01466529584256671612, -0.002851818597093459199 ) ) ;
#2621 = VERTEX_POINT ( 'NONE', #15419 ) ;
#2622 = ADVANCED_FACE ( 'NONE', ( #11039 ), #590, .F. ) ;
#2623 = EDGE_CURVE ( 'NONE', #13434, #3961, #17948, .T. ) ;
#2624 =( GEOMETRIC_REPRESENTATION_CONTEXT ( 3 ) GLOBAL_UNCERTAINTY_ASSIGNED_CONTEXT ( ( #11867 ) ) GLOBAL_UNIT_ASSIGNED_CONTEXT ( ( #18471, #18652, #13989 ) ) REPRESENTATION_CONTEXT ( 'NONE', 'WORKASPACE' ) );
#2625 = ORIENTED_EDGE ( 'NONE', *, *, #7208, .F. ) ;
#2626 = ORIENTED_EDGE ( 'NONE', *, *, #18781, .T. ) ;
#2627 = ORIENTED_EDGE ( 'NONE', *, *, #1071, .F. ) ;
#2628 = CYLINDRICAL_SURFACE ( 'NONE', #16295, 4.750000000000000000 ) ;
#2629 = VECTOR ( 'NONE', #12719, 1000.000000000000000 ) ;
#2630 = CARTESIAN_POINT ( 'NONE',  ( 2.697797270744669795, 12.89731672021094511, -3.226410068829295597 ) ) ;
#2631 = CARTESIAN_POINT ( 'NONE',  ( 16.56872352241294521, 0.004907101719994633009, -0.009207754980063766539 ) ) ;
#2632 = CARTESIAN_POINT ( 'NONE',  ( 0.3151930723728414985, 8.137566970826528134, -11.07033375389122831 ) ) ;
#2633 = EDGE_LOOP ( 'NONE', ( #1155, #10769, #13128, #16470 ) ) ;
#2634 = CARTESIAN_POINT ( 'NONE',  ( 2.705023505549862151, -12.88681800078730255, -3.294610156756031305 ) ) ;
#2635 = VECTOR ( 'NONE', #275, 1000.000000000000000 ) ;
#2636 = EDGE_CURVE ( 'NONE', #471, #6753, #821, .T. ) ;
#2637 = COLOUR_RGB ( '', 0.40784314, 0.44705882, 0.49803922) ;
#2638 = CARTESIAN_POINT ( 'NONE',  ( 16.56872352241294521, -0.007512283835805501873, -0.007240717549633963156 ) ) ;
#2639 = CARTESIAN_POINT ( 'NONE',  ( 1.454043889487796948, 7.500000000000062172, -13.09460583645960696 ) ) ;
#2640 = CARTESIAN_POINT ( 'NONE',  ( 0.3145734862173242274, -11.29227530924451273, 7.825584895511488170 ) ) ;
#2641 = LINE ( 'NONE', #18606, #10242 ) ;
#2642 = CIRCLE ( 'NONE', #13341, 0.5000000000000004441 ) ;
#2643 = PLANE ( 'NONE',  #442 ) ;
#2644 = DIRECTION ( 'NONE',  ( -1.000000000000000000, -0.000000000000000000, -0.000000000000000000 ) ) ;
#2645 = CARTESIAN_POINT ( 'NONE',  ( 0.3137051932979775248, -12.91601973349273891, 4.679953077377436266 ) ) ;
#2646 = ORIENTED_EDGE ( 'NONE', *, *, #11722, .T. ) ;
#2647 = AXIS2_PLACEMENT_3D ( 'NONE', #6461, #6559, #18480 ) ;
#2649 = ORIENTED_EDGE ( 'NONE', *, *, #9078, .F. ) ;
#2648 = CARTESIAN_POINT ( 'NONE',  ( 16.56872352241294521, -0.001821578298043862289, 0.01027347319884366027 ) ) ;
#2650 = CARTESIAN_POINT ( 'NONE',  ( 16.56822296793089322, -0.002414375228568327748, 0.009847136207496262617 ) ) ;
#2651 = CIRCLE ( 'NONE', #16093, 5.000000000000000888 ) ;
#2652 = ORIENTED_EDGE ( 'NONE', *, *, #14147, .F. ) ;
#2653 = DIRECTION ( 'NONE',  ( 0.000000000000000000, 0.000000000000000000, -1.000000000000000000 ) ) ;
#2654 = EDGE_CURVE ( 'NONE', #15726, #12603, #6937, .T. ) ;
#2655 = EDGE_LOOP ( 'NONE', ( #16966, #18392, #2535, #3703 ) ) ;
#2656 = CARTESIAN_POINT ( 'NONE',  ( 0.3939822652208134768, -3.598529276937167953, -13.34132036472940896 ) ) ;
#2657 = CARTESIAN_POINT ( 'NONE',  ( -6.453131650770636440, -2.715944631655204056, -12.00000000019080382 ) ) ;
#2658 = DIRECTION ( 'NONE',  ( -1.000000000000000000, -0.000000000000000000, -0.000000000000000000 ) ) ;
#2659 = ORIENTED_EDGE ( 'NONE', *, *, #17064, .F. ) ;
#2660 = CARTESIAN_POINT ( 'NONE',  ( 1.342453679581834924, -9.456403821038877666, 11.38190519890850183 ) ) ;
#2661 = AXIS2_PLACEMENT_3D ( 'NONE', #4448, #14665, #10468 ) ;
#2662 = EDGE_CURVE ( 'NONE', #15937, #17471, #13615, .T. ) ;
#2663 = CARTESIAN_POINT ( 'NONE',  ( 8.522092701127531811, 0.3779863304871219909, 6.946128462138597470 ) ) ;
#2664 = CARTESIAN_POINT ( 'NONE',  ( 1.846613052777651198, 12.43780859207240042, -0.3401093050882249558 ) ) ;
#2665 = DIRECTION ( 'NONE',  ( 0.000000000000000000, 0.000000000000000000, -1.000000000000000000 ) ) ;
#2666 = CARTESIAN_POINT ( 'NONE',  ( 0.3137051932979809665, -3.805684345189881856, 13.20008686438104739 ) ) ;
#2667 = DIRECTION ( 'NONE',  ( -0.5000000000000042188, 1.060575238724903710E-16, -0.8660254037844361541 ) ) ;
#2669 = EDGE_LOOP ( 'NONE', ( #14305, #3774, #4650, #17336 ) ) ;
#2668 = FACE_OUTER_BOUND ( 'NONE', #4674, .T. ) ;
#2670 = CARTESIAN_POINT ( 'NONE',  ( 1.977436885026095270, -10.21547824869579202, 11.52792723756318694 ) ) ;
#2671 = AXIS2_PLACEMENT_3D ( 'NONE', #1128, #7154, #1313 ) ;
#2672 = DIRECTION ( 'NONE',  ( -0.000000000000000000, -0.000000000000000000, 1.000000000000000000 ) ) ;
#2673 = EDGE_LOOP ( 'NONE', ( #12168, #18642, #6177, #14113, #15562, #12382, #1974, #16845, #13432, #10639, #9231, #4809, #18735, #17944, #10207, #18283, #18032, #11645, #6230, #9875, #7360, #7957, #15401, #1402, #14920, #10737, #6933, #9733, #2456, #16872, #1129, #17055, #14894, #17571, #1925, #11671, #10678, #15877, #17549, #12972, #4481, #2083, #9858, #5582, #8820, #12181, #10447, #12950, #7750, #2202, #1536, #2831, #12949, #12142, #2685, #8756, #5153, #2022, #16007, #15721, #2168, #10039, #3661, #16623 ) ) ;
#2674 = CARTESIAN_POINT ( 'NONE',  ( 8.522092701127531811, 1.786985377232127137, -6.722964936702079619 ) ) ;
#2675 = DIRECTION ( 'NONE',  ( 0.000000000000000000, -0.000000000000000000, 1.000000000000000000 ) ) ;
#2676 = EDGE_LOOP ( 'NONE', ( #1200, #12787 ) ) ;
#2677 = FACE_OUTER_BOUND ( 'NONE', #1853, .T. ) ;
#2678 = EDGE_CURVE ( 'NONE', #3393, #13262, #16400, .T. ) ;
#2679 = EDGE_CURVE ( 'NONE', #12041, #1137, #12547, .T. ) ;
#2680 = EDGE_CURVE ( 'NONE', #14205, #3723, #805, .T. ) ;
#2681 = CARTESIAN_POINT ( 'NONE',  ( 2.636624412715137922, -7.605649742761668719, 14.14563173255331741 ) ) ;
#2682 = CARTESIAN_POINT ( 'NONE',  ( 8.438534575730034959, -0.2320579683289648587, -6.862570336891078426 ) ) ;
#2683 = CARTESIAN_POINT ( 'NONE',  ( 1.861628059977341154, 7.751680370225533245, -9.751736252960284901 ) ) ;
#2684 = CARTESIAN_POINT ( 'NONE',  ( 0.000000000000000000, 0.000000000000000000, 0.000000000000000000 ) ) ;
#2685 = ORIENTED_EDGE ( 'NONE', *, *, #17500, .F. ) ;
#2686 = CARTESIAN_POINT ( 'NONE',  ( 0.4862570985993252548, 5.003653737315486794, 12.97920246947881395 ) ) ;
#2687 = CARTESIAN_POINT ( 'NONE',  ( 3.074695600507123761, 2.093687500612191776, -15.41438262616238575 ) ) ;
#2688 =( BOUNDED_SURFACE ( )  B_SPLINE_SURFACE ( 3, 1, ( 
 ( #15239, #9220 ),
 ( #2152, #10951 ),
 ( #14952, #12279 ),
 ( #7710, #6263 ) ),
 .UNSPECIFIED., .F., .F., .T. ) 
 B_SPLINE_SURFACE_WITH_KNOTS ( ( 4, 4 ),
 ( 2, 2 ),
 ( 0.000000000000000000, 1.000000000000000000 ),
 ( 0.000000000000000000, 1.000000000000000000 ),
 .UNSPECIFIED. ) 
 GEOMETRIC_REPRESENTATION_ITEM ( )  RATIONAL_B_SPLINE_SURFACE ( (
 ( 1.000000000000000000, 1.000000000000000000),
 ( 0.7792777138730160313, 0.9689936506012927220),
 ( 0.7792777138730160313, 0.9689936506012927220),
 ( 1.000000000000000000, 1.000000000000000000) ) ) 
 REPRESENTATION_ITEM ( '' )  SURFACE ( )  );
#2689 = CARTESIAN_POINT ( 'NONE',  ( -30.00000000000000355, -12.50000000000000178, 6.000000000000000000 ) ) ;
#2690 = CARTESIAN_POINT ( 'NONE',  ( 0.4754618798421167414, 10.80499583390513152, 8.775436892861154803 ) ) ;
#2691 = CARTESIAN_POINT ( 'NONE',  ( 2.500000000000000000, 0.000000000000000000, -3.000000000000000000 ) ) ;
#2692 = ORIENTED_EDGE ( 'NONE', *, *, #10424, .T. ) ;
#2693 = DIRECTION ( 'NONE',  ( 0.000000000000000000, 0.000000000000000000, 1.000000000000000000 ) ) ;
#2694 = CARTESIAN_POINT ( 'NONE',  ( 1.846138399168762101, -7.646096044339819819, -9.815003036200495856 ) ) ;
#2695 = EDGE_CURVE ( 'NONE', #9382, #15782, #9499, .T. ) ;
#2696 = ORIENTED_EDGE ( 'NONE', *, *, #17019, .T. ) ;
#2697 = ORIENTED_EDGE ( 'NONE', *, *, #9796, .T. ) ;
#2698 = CARTESIAN_POINT ( 'NONE',  ( 1.560000000000000053, 0.8660254037844389297, -1.500000000000000000 ) ) ;
#2699 = ORIENTED_EDGE ( 'NONE', *, *, #1825, .F. ) ;
#2700 = CARTESIAN_POINT ( 'NONE',  ( -27.50000000000000711, -12.50000000000000178, -7.071067811865460406 ) ) ;
#2701 = AXIS2_PLACEMENT_3D ( 'NONE', #16647, #16830, #5259 ) ;
#2702 = ORIENTED_EDGE ( 'NONE', *, *, #14408, .F. ) ;
#2703 = CARTESIAN_POINT ( 'NONE',  ( 3.950837973638676281, -6.316429227969562632, 13.10350451991838128 ) ) ;
#2704 = EDGE_CURVE ( 'NONE', #12932, #11277, #12193, .T. ) ;
#2705 = CARTESIAN_POINT ( 'NONE',  ( 1.846613052777651198, -10.26230975746754659, -7.035606253495426898 ) ) ;
#2706 = EDGE_CURVE ( 'NONE', #347, #18407, #1732, .T. ) ;
#2707 = FACE_OUTER_BOUND ( 'NONE', #10285, .T. ) ;
#2708 = CARTESIAN_POINT ( 'NONE',  ( 0.4862570985993235340, 13.89016912371017476, -0.7479633556562934604 ) ) ;
#2709 =( NAMED_UNIT ( * ) SI_UNIT ( $, .STERADIAN. ) SOLID_ANGLE_UNIT ( ) );
#2710 = DIRECTION ( 'NONE',  ( 1.000000000000000000, 0.000000000000000000, 0.000000000000000000 ) ) ;
#2711 = CARTESIAN_POINT ( 'NONE',  ( 0.3145729642390356351, -0.3065092323350255277, -13.73540280162741389 ) ) ;
#2712 = CIRCLE ( 'NONE', #2421, 5.000000000000000000 ) ;
#2713 = AXIS2_PLACEMENT_3D ( 'NONE', #16698, #1894, #5128 ) ;
#2714 = VECTOR ( 'NONE', #18374, 1000.000000000000000 ) ;
#2715 = CARTESIAN_POINT ( 'NONE',  ( 16.58200780006414732, -0.01115192838421470017, 0.0006320991582340292937 ) ) ;
#2716 = FACE_OUTER_BOUND ( 'NONE', #2222, .T. ) ;
#2717 = ORIENTED_EDGE ( 'NONE', *, *, #16502, .F. ) ;
#2718 = ORIENTED_EDGE ( 'NONE', *, *, #7759, .T. ) ;
#2719 = ORIENTED_EDGE ( 'NONE', *, *, #4263, .T. ) ;
#2720 = ORIENTED_EDGE ( 'NONE', *, *, #7923, .F. ) ;
#2721 = LINE ( 'NONE', #18787, #9566 ) ;
#2722 = CARTESIAN_POINT ( 'NONE',  ( 2.636624412714756005, -2.161493821597335607, 15.91454522070219113 ) ) ;
#2723 = CARTESIAN_POINT ( 'NONE',  ( 0.3150692679895986115, 8.199139630396166112, -11.02465386701219252 ) ) ;
#2724 = ORIENTED_EDGE ( 'NONE', *, *, #4872, .F. ) ;
#2725 = DIRECTION ( 'NONE',  ( -0.000000000000000000, 0.000000000000000000, 1.000000000000000000 ) ) ;
#2726 = LINE ( 'NONE', #11446, #15668 ) ;
#2727 = EDGE_CURVE ( 'NONE', #5155, #3, #5828, .T. ) ;
#2728 = CARTESIAN_POINT ( 'NONE',  ( 0.6925461861255360896, 7.499999999999999112, -14.36265820198533483 ) ) ;
#2729 = DIRECTION ( 'NONE',  ( -0.000000000000000000, -1.000000000000000000, -0.000000000000000000 ) ) ;
#2730 = CARTESIAN_POINT ( 'NONE',  ( 3.512766787570765548, -13.25664064834477429, 7.127386085302765295 ) ) ;
#2731 = CARTESIAN_POINT ( 'NONE',  ( 0.3137051932979792457, 11.37800749014131263, 7.698472063774513430 ) ) ;
#2732 = LINE ( 'NONE', #12968, #864 ) ;
#2733 = VERTEX_POINT ( 'NONE', #16767 ) ;
#2734 = VERTEX_POINT ( 'NONE', #3669 ) ;
#2735 = CARTESIAN_POINT ( 'NONE',  ( 3.950837973638676281, -14.41405733518061716, 1.958075594453740687 ) ) ;
#2736 = VECTOR ( 'NONE', #16072, 1000.000000000000114 ) ;
#2737 = ORIENTED_EDGE ( 'NONE', *, *, #7089, .F. ) ;
#2738 = EDGE_CURVE ( 'NONE', #11944, #14183, #18292, .T. ) ;
#2739 = ORIENTED_EDGE ( 'NONE', *, *, #15084, .T. ) ;
#2740 = DIRECTION ( 'NONE',  ( -1.000000000000000000, -0.000000000000000000, -0.000000000000000000 ) ) ;
#2741 = ORIENTED_EDGE ( 'NONE', *, *, #15320, .F. ) ;
#2742 = DIRECTION ( 'NONE',  ( 0.000000000000000000, -2.533398541561209262E-17, 1.000000000000000000 ) ) ;
#2743 = DIRECTION ( 'NONE',  ( 1.000000000000000000, 0.000000000000000000, 0.000000000000000000 ) ) ;
#2744 = LINE ( 'NONE', #1326, #5606 ) ;
#2745 = B_SPLINE_CURVE_WITH_KNOTS ( 'NONE', 3,
 ( #5075, #5357, #12437, #6713 ),
 .UNSPECIFIED., .F., .F.,
 ( 4, 4 ),
 ( 7.039312503357838248E-16, 0.002004993803841917561 ),
 .UNSPECIFIED. ) ;
#2746 = DIRECTION ( 'NONE',  ( 0.000000000000000000, -2.533398541561209262E-17, 1.000000000000000000 ) ) ;
#2747 = ORIENTED_EDGE ( 'NONE', *, *, #16564, .F. ) ;
#2748 = DIRECTION ( 'NONE',  ( 0.7561779333270775005, -0.6534392409364819798, -0.03481510524965015368 ) ) ;
#2749 = CARTESIAN_POINT ( 'NONE',  ( 0.3145729642390375225, -4.535980493005000724, -12.96842777670211611 ) ) ;
#2750 = CARTESIAN_POINT ( 'NONE',  ( 1.846955891736114852, 12.44001089941741611, -0.2634721419535633880 ) ) ;
#2751 = CARTESIAN_POINT ( 'NONE',  ( 2.747332970342022840, 16.12459247543626617, 2.705255688517901103 ) ) ;
#2752 = CYLINDRICAL_SURFACE ( 'NONE', #18758, 5.000000000000000888 ) ;
#2753 = FACE_OUTER_BOUND ( 'NONE', #18659, .T. ) ;
#2754 = APPLICATION_CONTEXT ( 'automotive_design' ) ;
#2755 = DIRECTION ( 'NONE',  ( 1.000000000000000000, 0.000000000000000000, 0.000000000000000000 ) ) ;
#2756 = EDGE_CURVE ( 'NONE', #11554, #16490, #4940, .T. ) ;
#2757 = CARTESIAN_POINT ( 'NONE',  ( 16.56679352167444819, -0.004277682826582317882, 0.008252760440870482092 ) ) ;
#2758 = ORIENTED_EDGE ( 'NONE', *, *, #11526, .F. ) ;
#2759 = CIRCLE ( 'NONE', #344, 0.2000000000000000944 ) ;
#2760 = CARTESIAN_POINT ( 'NONE',  ( -20.00000000000000000, -7.500000000000000888, -16.99999999999999645 ) ) ;
#2762 = EDGE_LOOP ( 'NONE', ( #16095, #331, #5318, #17520 ) ) ;
#2761 = FACE_BOUND ( 'NONE', #10743, .T. ) ;
#2763 = CARTESIAN_POINT ( 'NONE',  ( 0.3151926232592464627, -13.09050869763090219, -4.172630140040936908 ) ) ;
#2764 = ORIENTED_EDGE ( 'NONE', *, *, #5105, .T. ) ;
#2765 = CARTESIAN_POINT ( 'NONE',  ( 16.56822296793089322, -0.003834730849371946210, -0.009385634690642043892 ) ) ;
#2766 = CARTESIAN_POINT ( 'NONE',  ( 3.074695600507241444, -15.30693405987796751, 2.772091048739207864 ) ) ;
#2767 = B_SPLINE_CURVE_WITH_KNOTS ( 'NONE', 3,
 ( #15742, #6971, #6868, #7152, #15557, #5428 ),
 .UNSPECIFIED., .F., .F.,
 ( 4, 2, 4 ),
 ( 4.240893905418535831E-17, 0.0002014099069817285406, 0.0004028198139634146346 ),
 .UNSPECIFIED. ) ;
#2768 = ORIENTED_EDGE ( 'NONE', *, *, #12213, .F. ) ;
#2769 = FACE_OUTER_BOUND ( 'NONE', #11793, .T. ) ;
#2770 = DIRECTION ( 'NONE',  ( -1.000000000000000000, 0.000000000000000000, 0.000000000000000000 ) ) ;
#2771 = CIRCLE ( 'NONE', #9508, 4.750000000000000000 ) ;
#2772 = CARTESIAN_POINT ( 'NONE',  ( 0.4862570985993235340, -13.89016912371016943, -0.7479633556563904939 ) ) ;
#2773 = CARTESIAN_POINT ( 'NONE',  ( 1.562796894703937678, 0.000000000000000000, 0.000000000000000000 ) ) ;
#2774 = CARTESIAN_POINT ( 'NONE',  ( 1.845756295923359325, 11.97166802574126088, 3.386818134580099837 ) ) ;
#2775 = ORIENTED_EDGE ( 'NONE', *, *, #2206, .F. ) ;
#2776 = FILL_AREA_STYLE ('',( #7593 ) ) ;
#2777 = CARTESIAN_POINT ( 'NONE',  ( 1.560000000000000053, 0.8660254037844389297, 1.500000000000000000 ) ) ;
#2778 = CARTESIAN_POINT ( 'NONE',  ( 2.002547531651519996, -12.17374746633580784, 3.242439124566603326 ) ) ;
#2779 = CARTESIAN_POINT ( 'NONE',  ( 0.3720661004400040439, -0.7231997263363842965, -13.79610186261031046 ) ) ;
#2780 = CARTESIAN_POINT ( 'NONE',  ( -66.35602477868047799, -10.00000000000000888, -2.000000000000000000 ) ) ;
#2781 = CARTESIAN_POINT ( 'NONE',  ( 3.950837973638668288, 0.000000000000000000, 0.000000000000000000 ) ) ;
#2782 = EDGE_CURVE ( 'NONE', #4341, #11242, #10600, .T. ) ;
#2783 = VERTEX_POINT ( 'NONE', #2495 ) ;
#2784 = CARTESIAN_POINT ( 'NONE',  ( 0.3137051932979792457, 11.37800749014142276, -7.698472063774345564 ) ) ;
#2785 = LINE ( 'NONE', #9776, #7864 ) ;
#2786 = ORIENTED_EDGE ( 'NONE', *, *, #6420, .T. ) ;
#2787 = VERTEX_POINT ( 'NONE', #1170 ) ;
#2788 = CARTESIAN_POINT ( 'NONE',  ( 2.636624412715362631, -15.80357026013197519, 2.862162146984090327 ) ) ;
#2789 = ORIENTED_EDGE ( 'NONE', *, *, #129, .T. ) ;
#2790 = CARTESIAN_POINT ( 'NONE',  ( 16.56753206892534891, 0.008432171035096448775, -0.004368917149005366145 ) ) ;
#2791 = AXIS2_PLACEMENT_3D ( 'NONE', #5044, #7742, #9450 ) ;
#2792 = ORIENTED_EDGE ( 'NONE', *, *, #16862, .F. ) ;
#2793 = CARTESIAN_POINT ( 'NONE',  ( 0.4862570985993235340, 8.769551628660735787, 10.79774104611376373 ) ) ;
#2794 = DIRECTION ( 'NONE',  ( 0.000000000000000000, 0.000000000000000000, 1.000000000000000000 ) ) ;
#2795 = CARTESIAN_POINT ( 'NONE',  ( 0.3137051932979792457, -8.442169467526928983, 10.83767969834800127 ) ) ;
#2796 = CARTESIAN_POINT ( 'NONE',  ( 0.3170788640506440603, 0.1533108587038062576, -13.74111462631963398 ) ) ;
#2797 =( BOUNDED_SURFACE ( )  B_SPLINE_SURFACE ( 3, 1, ( 
 ( #1570, #14752 ),
 ( #11801, #3377 ),
 ( #7413, #5960 ),
 ( #17633, #1663 ) ),
 .UNSPECIFIED., .F., .F., .T. ) 
 B_SPLINE_SURFACE_WITH_KNOTS ( ( 4, 4 ),
 ( 2, 2 ),
 ( 0.000000000000000000, 1.000000000000000000 ),
 ( 0.000000000000000000, 1.000000000000000000 ),
 .UNSPECIFIED. ) 
 GEOMETRIC_REPRESENTATION_ITEM ( )  RATIONAL_B_SPLINE_SURFACE ( (
 ( 1.000000000000000000, 1.000000000000000000),
 ( 0.7792777138730158093, 0.9689936506012928330),
 ( 0.7792777138730158093, 0.9689936506012928330),
 ( 1.000000000000000000, 1.000000000000000000) ) ) 
 REPRESENTATION_ITEM ( '' )  SURFACE ( )  );
#2798 = DIRECTION ( 'NONE',  ( -1.000000000000000000, 0.000000000000000000, 0.000000000000000000 ) ) ;
#2799 = CARTESIAN_POINT ( 'NONE',  ( 1.845756295923359547, 4.296776483139476355, 11.67600463554274626 ) ) ;
#2800 = CARTESIAN_POINT ( 'NONE',  ( 0.3151926232592482946, -13.04305446098359056, 4.318679262939574492 ) ) ;
#2801 = CARTESIAN_POINT ( 'NONE',  ( 16.56782317627811096, -0.009439921864426870785, 0.002708056627498742989 ) ) ;
#2802 = ADVANCED_FACE ( 'NONE', ( #12634 ), #18845, .F. ) ;
#2803 = VERTEX_POINT ( 'NONE', #983 ) ;
#2804 = EDGE_CURVE ( 'NONE', #2807, #819, #7009, .T. ) ;
#2805 = VERTEX_POINT ( 'NONE', #8433 ) ;
#2806 = AXIS2_PLACEMENT_3D ( 'NONE', #2197, #12505, #6691 ) ;
#2807 = VERTEX_POINT ( 'NONE', #6022 ) ;
#2808 = ORIENTED_EDGE ( 'NONE', *, *, #3930, .T. ) ;
#2809 = ORIENTED_EDGE ( 'NONE', *, *, #17661, .F. ) ;
#2810 = CARTESIAN_POINT ( 'NONE',  ( 3.950837973638676281, 13.10350451991840615, 6.316429227969512894 ) ) ;
#2811 = CARTESIAN_POINT ( 'NONE',  ( 16.56753206892534891, -0.008432171035096417550, 0.004368917149005420789 ) ) ;
#2812 = DIRECTION ( 'NONE',  ( -0.000000000000000000, -0.000000000000000000, -1.000000000000000000 ) ) ;
#2813 = EDGE_LOOP ( 'NONE', ( #12751, #16140 ) ) ;
#2814 = DIRECTION ( 'NONE',  ( 0.000000000000000000, 0.000000000000000000, 1.000000000000000000 ) ) ;
#2815 = CARTESIAN_POINT ( 'NONE',  ( 3.512766787570727356, 6.535475144497194577, -13.55823433651945464 ) ) ;
#2816 = CARTESIAN_POINT ( 'NONE',  ( 5.324905852943008000, 7.499999999999999112, -16.88120503408576312 ) ) ;
#2817 = CARTESIAN_POINT ( 'NONE',  ( 16.56822296793089322, -0.005339139727952723832, 0.008619100080559757848 ) ) ;
#2818 = CARTESIAN_POINT ( 'NONE',  ( 0.3145729642390390768, -10.93201268464378373, 8.321438378985218876 ) ) ;
#2819 = AXIS2_PLACEMENT_3D ( 'NONE', #1898, #3692, #7831 ) ;
#2820 = CARTESIAN_POINT ( 'NONE',  ( 16.57778382496167424, -0.001819584982832002807, 0.01482878558584568851 ) ) ;
#2821 = CARTESIAN_POINT ( 'NONE',  ( 2.123976203522053297, 14.31368049382969687, 6.261444813538606269 ) ) ;
#2822 = CARTESIAN_POINT ( 'NONE',  ( 16.56822296793089322, 0.009847136207495308519, -0.002414375228568875487 ) ) ;
#2823 = CARTESIAN_POINT ( 'NONE',  ( 1.847168016377981781, -3.666915430942684129, 11.89018175117593934 ) ) ;
#2824 = ORIENTED_EDGE ( 'NONE', *, *, #7779, .T. ) ;
#2825 = ORIENTED_EDGE ( 'NONE', *, *, #13866, .F. ) ;
#2826 = ORIENTED_EDGE ( 'NONE', *, *, #12336, .F. ) ;
#2827 = EDGE_CURVE ( 'NONE', #12087, #16455, #10055, .T. ) ;
#2828 = ORIENTED_EDGE ( 'NONE', *, *, #509, .F. ) ;
#2829 = CARTESIAN_POINT ( 'NONE',  ( 16.58200780006414732, 0.01080144354108992025, -0.002844973367390922145 ) ) ;
#2830 = VECTOR ( 'NONE', #196, 1000.000000000000000 ) ;
#2831 = ORIENTED_EDGE ( 'NONE', *, *, #10308, .T. ) ;
#2832 = CARTESIAN_POINT ( 'NONE',  ( 2.002547531651519996, 3.242439124566821818, -12.17374746633574745 ) ) ;
#2833 = CARTESIAN_POINT ( 'NONE',  ( 2.002547531651519996, -7.942910686618240845, 9.778737580845669797 ) ) ;
#2834 = DIRECTION ( 'NONE',  ( 0.000000000000000000, 0.000000000000000000, 1.000000000000000000 ) ) ;
#2835 = DIRECTION ( 'NONE',  ( 0.7635533937278214944, 0.2197766120036505344, -0.6071939193889570596 ) ) ;
#2836 = ORIENTED_EDGE ( 'NONE', *, *, #9238, .F. ) ;
#2837 = CARTESIAN_POINT ( 'NONE',  ( 16.58200780006414732, -0.01115192838421568723, -0.0006320991582349211584 ) ) ;
#2838 = DIRECTION ( 'NONE',  ( 0.000000000000000000, 1.000000000000000000, 1.224646799147353454E-16 ) ) ;
#2839 = CARTESIAN_POINT ( 'NONE',  ( 1.847412631396503579, 12.44294644888238999, 0.04315047898439477309 ) ) ;
#2840 = CARTESIAN_POINT ( 'NONE',  ( 0.3170788640506440603, 7.952793437297573931, 11.20690911610906326 ) ) ;
#2841 = CARTESIAN_POINT ( 'NONE',  ( 0.3939822652208126996, -8.678192463540247203, 10.75310269629518700 ) ) ;
#2842 = DIRECTION ( 'NONE',  ( -1.000000000000000000, -2.081668171172168513E-16, 1.826842780715651273E-15 ) ) ;
#2843 = DIRECTION ( 'NONE',  ( 0.000000000000000000, 0.000000000000000000, 1.000000000000000000 ) ) ;
#2844 = ORIENTED_EDGE ( 'NONE', *, *, #9940, .F. ) ;
#2845 = AXIS2_PLACEMENT_3D ( 'NONE', #3105, #14681, #10686 ) ;
#2846 = VECTOR ( 'NONE', #8489, 1000.000000000000114 ) ;
#2847 = PRODUCT_DEFINITION ( 'UNKNOWN', '', #12632, #13642 ) ;
#2848 = EDGE_CURVE ( 'NONE', #7476, #18002, #17000, .T. ) ;
#2849 = CARTESIAN_POINT ( 'NONE',  ( 2.636624412714994037, -14.46769361191274328, -6.973567714907344950 ) ) ;
#2851 = ORIENTED_EDGE ( 'NONE', *, *, #7066, .T. ) ;
#2850 = DIRECTION ( 'NONE',  ( -0.000000000000000000, -0.000000000000000000, -1.000000000000000000 ) ) ;
#2852 = DIRECTION ( 'NONE',  ( -0.7635533937278214944, 0.3620487483322560873, -0.5347026451755899634 ) ) ;
#2853 = EDGE_CURVE ( 'NONE', #14774, #9063, #7865, .T. ) ;
#2854 = CARTESIAN_POINT ( 'NONE',  ( 0.3095370825347224519, -12.91933430393611282, 4.681152801286110332 ) ) ;
#2855 = VERTEX_POINT ( 'NONE', #14354 ) ;
#2856 = LINE ( 'NONE', #2674, #13569 ) ;
#2857 = CARTESIAN_POINT ( 'NONE',  ( 3.669726844813488764, -7.499999999999743316, -13.21471411064825396 ) ) ;
#2858 = VERTEX_POINT ( 'NONE', #14165 ) ;
#2859 = CARTESIAN_POINT ( 'NONE',  ( 0.3095370825347224519, 13.20347358821914519, 3.806662003783459092 ) ) ;
#2860 = DIRECTION ( 'NONE',  ( -1.000000000000000000, -0.000000000000000000, -0.000000000000000000 ) ) ;
#2861 = DIRECTION ( 'NONE',  ( -0.000000000000000000, -0.000000000000000000, 1.000000000000000000 ) ) ;
#2862 = CARTESIAN_POINT ( 'NONE',  ( 0.3151928479966097374, -6.943324943027912228E-05, -13.73922861026898623 ) ) ;
#2863 = AXIS2_PLACEMENT_3D ( 'NONE', #6424, #1934, #13683 ) ;
#2864 = AXIS2_PLACEMENT_3D ( 'NONE', #6448, #5187, #9308 ) ;
#2865 = EDGE_CURVE ( 'NONE', #9201, #10624, #18562, .T. ) ;
#2866 = ORIENTED_EDGE ( 'NONE', *, *, #1916, .F. ) ;
#2867 = B_SPLINE_CURVE_WITH_KNOTS ( 'NONE', 3,
 ( #6900, #18641, #6999, #10139 ),
 .UNSPECIFIED., .F., .F.,
 ( 4, 4 ),
 ( 1.582786644015060892E-17, 0.003005512676784847896 ),
 .UNSPECIFIED. ) ;
#2868 = AXIS2_PLACEMENT_3D ( 'NONE', #8380, #8294, #14484 ) ;
#2869 = DIRECTION ( 'NONE',  ( -0.000000000000000000, 1.000000000000000000, -0.000000000000000000 ) ) ;
#2870 = CARTESIAN_POINT ( 'NONE',  ( 2.123976203522053741, 15.54801196254787143, -1.531817366691807125 ) ) ;
#2871 = CARTESIAN_POINT ( 'NONE',  ( 0.000000000000000000, -2.500000000000000444, -22.00000000000000000 ) ) ;
#2872 = DIRECTION ( 'NONE',  ( 0.4246593920385850485, 0.1376957914266804250, -0.8948208031649687033 ) ) ;
#2873 = AXIS2_PLACEMENT_3D ( 'NONE', #14246, #14422, #1332 ) ;
#2874 = ORIENTED_EDGE ( 'NONE', *, *, #9936, .T. ) ;
#2875 = CARTESIAN_POINT ( 'NONE',  ( 3.664313757352975820, -10.50730552161225972, -9.645155442698879256 ) ) ;
#2876 = DIRECTION ( 'NONE',  ( 0.000000000000000000, 0.000000000000000000, 1.000000000000000000 ) ) ;
#2877 = CIRCLE ( 'NONE', #12359, 1.500000000000000000 ) ;
#2878 = EDGE_LOOP ( 'NONE', ( #15032, #425, #13147, #2999 ) ) ;
#2879 = VECTOR ( 'NONE', #2532, 1000.000000000000114 ) ;
#2880 = ORIENTED_EDGE ( 'NONE', *, *, #18640, .T. ) ;
#2881 = CARTESIAN_POINT ( 'NONE',  ( 0.4754618798421171855, -10.80499583390519192, 8.775436892861074867 ) ) ;
#2882 = VERTEX_POINT ( 'NONE', #18469 ) ;
#2883 = LINE ( 'NONE', #13129, #9817 ) ;
#2884 = ORIENTED_EDGE ( 'NONE', *, *, #17544, .F. ) ;
#2885 = CARTESIAN_POINT ( 'NONE',  ( 0.4862570985993252548, 11.67702470553365401, 7.559321496869467971 ) ) ;
#2886 = CYLINDRICAL_SURFACE ( 'NONE', #12093, 2.500000000000000000 ) ;
#2887 = CARTESIAN_POINT ( 'NONE',  ( 1.847372867223022297, -10.00438561114518521, -7.398914411685100667 ) ) ;
#2888 = EDGE_CURVE ( 'NONE', #257, #16346, #7205, .T. ) ;
#2889 = AXIS2_PLACEMENT_3D ( 'NONE', #9128, #3482, #10854 ) ;
#2890 = CARTESIAN_POINT ( 'NONE',  ( 0.000000000000000000, 0.000000000000000000, -3.000000000000000000 ) ) ;
#2891 = CARTESIAN_POINT ( 'NONE',  ( 22.75000000000000000, 2.789133085058097101E-16, -2.055000000000000160 ) ) ;
#2892 = AXIS2_PLACEMENT_3D ( 'NONE', #15262, #831, #14097 ) ;
#2893 = CARTESIAN_POINT ( 'NONE',  ( 3.950837973638675393, -2.591948120961912849, 14.31366178983252446 ) ) ;
#2894 = CARTESIAN_POINT ( 'NONE',  ( 0.3137051932979792457, 7.698472063774471685, 11.37800749014133928 ) ) ;
#2895 = CARTESIAN_POINT ( 'NONE',  ( -53.40568638168567617, 9.314871387272408043, 3.000000000000000000 ) ) ;
#2896 = ORIENTED_EDGE ( 'NONE', *, *, #7882, .T. ) ;
#2897 = VERTEX_POINT ( 'NONE', #1069 ) ;
#2898 = ORIENTED_EDGE ( 'NONE', *, *, #4126, .T. ) ;
#2899 = ORIENTED_EDGE ( 'NONE', *, *, #6393, .T. ) ;
#2900 = CIRCLE ( 'NONE', #2326, 2.499999999999995115 ) ;
#2901 = ORIENTED_EDGE ( 'NONE', *, *, #373, .F. ) ;
#2902 = AXIS2_PLACEMENT_3D ( 'NONE', #12160, #10430, #8893 ) ;
#2903 = LINE ( 'NONE', #7339, #14750 ) ;
#2904 = CARTESIAN_POINT ( 'NONE',  ( 1.845756295923363099, -0.4783934145701149721, -12.43231724724606835 ) ) ;
#2905 = CARTESIAN_POINT ( 'NONE',  ( 1.254255976357087521, 11.25336128106905420, 9.426444230096484134 ) ) ;
#2906 = EDGE_LOOP ( 'NONE', ( #5067, #420, #18863, #7212 ) ) ;
#2907 = CARTESIAN_POINT ( 'NONE',  ( 3.950837973638675393, -14.31366178983251380, -2.591948120961955926 ) ) ;
#2908 = ADVANCED_FACE ( 'NONE', ( #14447 ), #3970, .F. ) ;
#2909 = EDGE_CURVE ( 'NONE', #4576, #11470, #8755, .T. ) ;
#2910 = CARTESIAN_POINT ( 'NONE',  ( 1.560000000000000053, 0.000000000000000000, 0.000000000000000000 ) ) ;
#2911 = ADVANCED_FACE ( 'NONE', ( #15509 ), #5378, .T. ) ;
#2912 = FACE_OUTER_BOUND ( 'NONE', #1204, .T. ) ;
#2913 = CARTESIAN_POINT ( 'NONE',  ( 16.57778382496167424, 0.01354073047775893567, -0.006312874906843913766 ) ) ;
#2914 = CARTESIAN_POINT ( 'NONE',  ( 1.846138399168762101, -10.30487220521574976, 6.971848976710974810 ) ) ;
#2915 = DIRECTION ( 'NONE',  ( 1.000000000000000000, 0.000000000000000000, 0.000000000000000000 ) ) ;
#2916 = CARTESIAN_POINT ( 'NONE',  ( 0.8740779401508875779, -3.609949156401464965, 13.83508928787437142 ) ) ;
#2917 = DIRECTION ( 'NONE',  ( 0.000000000000000000, -1.000000000000000000, 0.000000000000000000 ) ) ;
#2918 = VECTOR ( 'NONE', #16196, 1000.000000000000000 ) ;
#2919 = PRESENTATION_LAYER_ASSIGNMENT (  '', '', ( #3857 ) ) ;
#2920 = CARTESIAN_POINT ( 'NONE',  ( 1.846822687350019088, 7.075150813727119292, 10.23524390843941845 ) ) ;
#2921 = ORIENTED_EDGE ( 'NONE', *, *, #4580, .F. ) ;
#2922 = PRODUCT_DEFINITION_SHAPE ( 'NONE', 'NONE',  #18917 ) ;
#2923 = EDGE_CURVE ( 'NONE', #17620, #12792, #10632, .T. ) ;
#2924 = ORIENTED_EDGE ( 'NONE', *, *, #15352, .F. ) ;
#2925 = ORIENTED_EDGE ( 'NONE', *, *, #18359, .F. ) ;
#2926 = CIRCLE ( 'NONE', #4178, 14.54644660717763927 ) ;
#2927 = VERTEX_POINT ( 'NONE', #10804 ) ;
#2928 = DIRECTION ( 'NONE',  ( 0.000000000000000000, 0.000000000000000000, 1.000000000000000000 ) ) ;
#2929 = VECTOR ( 'NONE', #1389, 1000.000000000000000 ) ;
#2930 = PRESENTATION_LAYER_ASSIGNMENT (  '', '', ( #4169 ) ) ;
#2931 = ORIENTED_EDGE ( 'NONE', *, *, #722, .T. ) ;
#2932 = LINE ( 'NONE', #9923, #14944 ) ;
#2933 = DIRECTION ( 'NONE',  ( 1.000000000000000000, -2.775557561562892929E-15, 0.000000000000000000 ) ) ;
#2934 = CARTESIAN_POINT ( 'NONE',  ( 2.002547531651519996, 4.532360870844327039, 11.75462648437103752 ) ) ;
#2935 = AXIS2_PLACEMENT_3D ( 'NONE', #13091, #5626, #12899 ) ;
#2936 = CARTESIAN_POINT ( 'NONE',  ( 1.846613052777650976, -0.3401093050880946711, -12.43780859207240219 ) ) ;
#2937 = ORIENTED_EDGE ( 'NONE', *, *, #6465, .F. ) ;
#2938 = CARTESIAN_POINT ( 'NONE',  ( 0.3095370825347224519, 13.20347358821914519, 3.806662003783459092 ) ) ;
#2939 = AXIS2_PLACEMENT_3D ( 'NONE', #7030, #12844, #11425 ) ;
#2940 = CARTESIAN_POINT ( 'NONE',  ( 1.918918678667044686, -10.48466773720556766, -6.832809802519125064 ) ) ;
#2941 = CARTESIAN_POINT ( 'NONE',  ( 3.950837973638676281, -10.05648675950133963, 10.51028938476214059 ) ) ;
#2942 = DIRECTION ( 'NONE',  ( 0.000000000000000000, 0.000000000000000000, 1.000000000000000000 ) ) ;
#2943 = CARTESIAN_POINT ( 'NONE',  ( 2.002547531651519996, 3.242439124566821818, -12.17374746633574745 ) ) ;
#2944 = ADVANCED_FACE ( 'NONE', ( #16350 ), #2502, .F. ) ;
#2945 = VECTOR ( 'NONE', #18300, 1000.000000000000114 ) ;
#2946 = AXIS2_PLACEMENT_3D ( 'NONE', #8725, #14838, #11978 ) ;
#2947 = PRESENTATION_LAYER_ASSIGNMENT (  '', '', ( #10609 ) ) ;
#2948 = CYLINDRICAL_SURFACE ( 'NONE', #15654, 5.000000000000000888 ) ;
#2949 = VERTEX_POINT ( 'NONE', #2015 ) ;
#2950 = CARTESIAN_POINT ( 'NONE',  ( 0.8740764193767813772, -12.04241474977994208, 7.708542792189371440 ) ) ;
#2952 = ORIENTED_EDGE ( 'NONE', *, *, #922, .F. ) ;
#2951 = CARTESIAN_POINT ( 'NONE',  ( 1.321128355694181398E-14, -8.013167318348353163, 12.51316734529529562 ) ) ;
#2953 = CARTESIAN_POINT ( 'NONE',  ( 2.002547531651519996, 12.17374746633578475, 3.242439124566693476 ) ) ;
#2954 = ADVANCED_FACE ( 'NONE', ( #16249 ), #3131, .T. ) ;
#2955 = CARTESIAN_POINT ( 'NONE',  ( 16.56753206892534891, -0.008432171035096412345, -0.004368917149004214288 ) ) ;
#2956 = ORIENTED_EDGE ( 'NONE', *, *, #18476, .F. ) ;
#2957 = CARTESIAN_POINT ( 'NONE',  ( 0.3148208552358935930, 4.026279359288611026, -13.13564827777585187 ) ) ;
#2958 = CARTESIAN_POINT ( 'NONE',  ( 2.576507258269559397, -7.499999999999741540, -13.18245040793293121 ) ) ;
#2959 = ORIENTED_EDGE ( 'NONE', *, *, #3458, .F. ) ;
#2960 = CARTESIAN_POINT ( 'NONE',  ( 0.4754618798421162973, 7.564402563418467729, 11.68486377711969304 ) ) ;
#2961 =( LENGTH_UNIT ( ) NAMED_UNIT ( * ) SI_UNIT ( .MILLI., .METRE. ) );
#2962 = CARTESIAN_POINT ( 'NONE',  ( -31.48433267924924550, 17.77350098112614418, 3.000000000000000000 ) ) ;
#2963 = DIRECTION ( 'NONE',  ( -1.000000000000000000, -0.000000000000000000, -0.000000000000000000 ) ) ;
#2964 = B_SPLINE_CURVE_WITH_KNOTS ( 'NONE', 3,
 ( #15830, #5502, #8854, #2905, #11724, #16123 ),
 .UNSPECIFIED., .F., .F.,
 ( 4, 2, 4 ),
 ( 0.000000000000000000, 0.001656992708821599649, 0.003313985417643199299 ),
 .UNSPECIFIED. ) ;
#2965 = CIRCLE ( 'NONE', #8473, 3.999999999999993339 ) ;
#2966 = DIRECTION ( 'NONE',  ( 0.000000000000000000, 0.000000000000000000, -1.000000000000000000 ) ) ;
#2967 = CARTESIAN_POINT ( 'NONE',  ( 0.3939875929385612263, 10.75308190953755982, -8.678227324501007089 ) ) ;
#2968 = B_SPLINE_CURVE_WITH_KNOTS ( 'NONE', 3,
 ( #5668, #11428, #8370, #6948, #8283, #3972 ),
 .UNSPECIFIED., .F., .F.,
 ( 4, 2, 4 ),
 ( 3.490137563248181679E-18, 0.0002017457492448096685, 0.0004034914984896158133 ),
 .UNSPECIFIED. ) ;
#2969 = EDGE_CURVE ( 'NONE', #6750, #3366, #672, .T. ) ;
#2970 = CARTESIAN_POINT ( 'NONE',  ( 0.3720661004400040439, -4.951033743989553315, -12.89739157014198057 ) ) ;
#2971 = DIRECTION ( 'NONE',  ( -1.000000000000000000, 0.000000000000000000, 0.000000000000000000 ) ) ;
#2972 = LINE ( 'NONE', #8819, #9982 ) ;
#2973 = ORIENTED_EDGE ( 'NONE', *, *, #875, .F. ) ;
#2974 = CARTESIAN_POINT ( 'NONE',  ( 1.861706995891667882, 4.359009869687244354, 11.66987142852985748 ) ) ;
#2975 = CARTESIAN_POINT ( 'NONE',  ( 16.56679352167444819, 0.006526964904752344775, -0.006618561353600113835 ) ) ;
#2976 = ORIENTED_EDGE ( 'NONE', *, *, #10158, .T. ) ;
#2977 = ADVANCED_FACE ( 'NONE', ( #6312 ), #4479, .F. ) ;
#2978 = EDGE_LOOP ( 'NONE', ( #8962, #14482, #14596, #6626 ) ) ;
#2979 = FACE_OUTER_BOUND ( 'NONE', #18901, .T. ) ;
#2980 = ORIENTED_EDGE ( 'NONE', *, *, #15931, .T. ) ;
#2981 = CARTESIAN_POINT ( 'NONE',  ( 2.747332970342022840, 11.66639548242807578, 11.45495994260722306 ) ) ;
#2982 = ORIENTED_EDGE ( 'NONE', *, *, #3153, .T. ) ;
#2983 = CARTESIAN_POINT ( 'NONE',  ( 16.56822296793089322, 0.003834730849370841625, -0.009385634690641637967 ) ) ;
#2984 = CARTESIAN_POINT ( 'NONE',  ( 16.58200780006414732, 0.007066318000006001528, -0.008650561019685833880 ) ) ;
#2985 = CARTESIAN_POINT ( 'NONE',  ( 0.3132635586635978409, 13.72732610560088773, -0.5277914263193584921 ) ) ;
#2986 = CARTESIAN_POINT ( 'NONE',  ( 1.845755665166727066, -4.296872077620760066, 11.67596932341233007 ) ) ;
#2987 = CARTESIAN_POINT ( 'NONE',  ( 0.4754618798421162973, 12.98792082933651493, -5.007009103465114741 ) ) ;
#2988 = CARTESIAN_POINT ( 'NONE',  ( 3.686287386450715076E-15, -27.00000000000000000, 25.01316734529526187 ) ) ;
#2989 =( NAMED_UNIT ( * ) SI_UNIT ( $, .STERADIAN. ) SOLID_ANGLE_UNIT ( ) );
#2990 = DIRECTION ( 'NONE',  ( 0.000000000000000000, 0.000000000000000000, -1.000000000000000000 ) ) ;
#2991 = CARTESIAN_POINT ( 'NONE',  ( 0.4754618798421171855, 3.583352865732860604, -13.45049478164055756 ) ) ;
#2992 = DIRECTION ( 'NONE',  ( 1.000000000000000000, 0.000000000000000000, 0.000000000000000000 ) ) ;
#2993 = CARTESIAN_POINT ( 'NONE',  ( 16.58200780006414732, -0.002844973367390960309, -0.01080144354108991157 ) ) ;
#2994 = EDGE_CURVE ( 'NONE', #4199, #666, #18594, .T. ) ;
#2995 = ORIENTED_EDGE ( 'NONE', *, *, #680, .F. ) ;
#2996 = CARTESIAN_POINT ( 'NONE',  ( 1.846138399168762101, -6.971848976710933954, -10.30487220521577818 ) ) ;
#2997 = ORIENTED_EDGE ( 'NONE', *, *, #3840, .T. ) ;
#2998 = ADVANCED_FACE ( 'NONE', ( #291 ), #8996, .F. ) ;
#2999 = ORIENTED_EDGE ( 'NONE', *, *, #18071, .F. ) ;
#3000 = ORIENTED_EDGE ( 'NONE', *, *, #7475, .F. ) ;
#3001 = ORIENTED_EDGE ( 'NONE', *, *, #6952, .F. ) ;
#3002 = CARTESIAN_POINT ( 'NONE',  ( 1.861628059977343597, -9.751736252960316875, -7.751680370225499495 ) ) ;
#3003 = CARTESIAN_POINT ( 'NONE',  ( 2.320521194583477165, -6.542541239686160637, -14.32454473829993447 ) ) ;
#3004 = CARTESIAN_POINT ( 'NONE',  ( 3.950837973638677170, -1.958075594453692503, -14.41405733518062959 ) ) ;
#3005 = EDGE_LOOP ( 'NONE', ( #15141, #81, #4937, #1625 ) ) ;
#3006 = CARTESIAN_POINT ( 'NONE',  ( 3.377929128793393687, 1.296196549818942501, 13.92579934231096317 ) ) ;
#3007 = DIRECTION ( 'NONE',  ( -0.7635533937278216055, 0.1790966170214010056, -0.6204116510013458763 ) ) ;
#3008 = DIRECTION ( 'NONE',  ( -0.7635533937278216055, 0.02138673900301891681, 0.6453904417649388714 ) ) ;
#3009 = CARTESIAN_POINT ( 'NONE',  ( 19.99999999999999645, 20.00000000000000000, 0.000000000000000000 ) ) ;
#3010 = CARTESIAN_POINT ( 'NONE',  ( 2.636624412715435462, -15.80357026013316712, -2.862162146983298516 ) ) ;
#3011 = AXIS2_PLACEMENT_3D ( 'NONE', #14683, #5788, #4368 ) ;
#3012 = CARTESIAN_POINT ( 'NONE',  ( 2.636624412714242194, 14.46769361191244485, 6.973567714906650394 ) ) ;
#3013 = DIRECTION ( 'NONE',  ( 6.938893903907227392E-16, 0.000000000000000000, 1.000000000000000000 ) ) ;
#3014 = CARTESIAN_POINT ( 'NONE',  ( 16.57605080000000086, 6.799999999999999822, 1.500000000000000000 ) ) ;
#3015 = CARTESIAN_POINT ( 'NONE',  ( 0.4862570985993252548, 13.44146924561381162, 3.580942890621718888 ) ) ;
#3016 = AXIS2_PLACEMENT_3D ( 'NONE', #6543, #17924, #13612 ) ;
#3017 = VERTEX_POINT ( 'NONE', #7661 ) ;
#3018 = ORIENTED_EDGE ( 'NONE', *, *, #7834, .F. ) ;
#3019 = B_SPLINE_CURVE_WITH_KNOTS ( 'NONE', 3,
 ( #4046, #9859, #15695, #8536, #5555, #2597, #11411 ),
 .UNSPECIFIED., .F., .F.,
 ( 4, 3, 4 ),
 ( 1.843143693225357538E-18, 0.0002299804304191480943, 0.0004168119862255878537 ),
 .UNSPECIFIED. ) ;
#3020 = ADVANCED_FACE ( 'NONE', ( #385 ), #11791, .F. ) ;
#3021 = ORIENTED_EDGE ( 'NONE', *, *, #3475, .T. ) ;
#3022 = ORIENTED_EDGE ( 'NONE', *, *, #2865, .T. ) ;
#3023 = FACE_OUTER_BOUND ( 'NONE', #6790, .T. ) ;
#3024 = ORIENTED_EDGE ( 'NONE', *, *, #14053, .T. ) ;
#3025 = CARTESIAN_POINT ( 'NONE',  ( 0.3307726912345205217, -11.46720933246392882, -7.596084275799019458 ) ) ;
#3026 = LINE ( 'NONE', #17381, #6256 ) ;
#3027 = CARTESIAN_POINT ( 'NONE',  ( 16.57210152137263393, -0.008007331252333342933, 0.01214401161737632510 ) ) ;
#3028 = CARTESIAN_POINT ( 'NONE',  ( 1.847168016377982003, -0.1868244120188694568, -12.44137401948661292 ) ) ;
#3029 = VERTEX_POINT ( 'NONE', #16999 ) ;
#3030 = CARTESIAN_POINT ( 'NONE',  ( -6.538348415311014072, 7.499999999999999112, -16.99999999999999645 ) ) ;
#3031 = CARTESIAN_POINT ( 'NONE',  ( 0.3151926232592538457, -4.318679262939536301, -13.04305446098360122 ) ) ;
#3032 = CARTESIAN_POINT ( 'NONE',  ( 1.846138399168762101, 3.446241763653166590, -11.95493567637846866 ) ) ;
#3033 = CARTESIAN_POINT ( 'NONE',  ( 1.254009781012409341, 13.61532727684501509, -5.487405433548977030 ) ) ;
#3034 =( NAMED_UNIT ( * ) PLANE_ANGLE_UNIT ( ) SI_UNIT ( $, .RADIAN. ) );
#3035 = B_SPLINE_CURVE_WITH_KNOTS ( 'NONE', 3,
 ( #13045, #5772, #17741, #17644 ),
 .UNSPECIFIED., .F., .F.,
 ( 4, 4 ),
 ( 5.784724088816010014E-17, 0.002004993803842651783 ),
 .UNSPECIFIED. ) ;
#3036 = CARTESIAN_POINT ( 'NONE',  ( 2.949999999999999734, 3.061616997868382648E-16, -2.499999999999999556 ) ) ;
#3037 = ORIENTED_EDGE ( 'NONE', *, *, #4714, .T. ) ;
#3038 = B_SPLINE_CURVE_WITH_KNOTS ( 'NONE', 3,
 ( #12645, #5387, #17050, #6921 ),
 .UNSPECIFIED., .F., .F.,
 ( 4, 4 ),
 ( 1.684670163748776910E-17, 0.003005512676784852233 ),
 .UNSPECIFIED. ) ;
#3039 = CARTESIAN_POINT ( 'NONE',  ( 3.950837973638675393, 2.591948120961804936, 14.31366178983254578 ) ) ;
#3041 = EDGE_LOOP ( 'NONE', ( #9922, #15624, #14342, #4151 ) ) ;
#3040 = CARTESIAN_POINT ( 'NONE',  ( 0.3151926232592474064, 0.07678256780557664307, 13.73922722301401578 ) ) ;
#3042 = EDGE_CURVE ( 'NONE', #17275, #4049, #9930, .T. ) ;
#3043 = CARTESIAN_POINT ( 'NONE',  ( 0.3095370825347224519, -0.4597470195089233824, -13.73357284481725316 ) ) ;
#3044 = EDGE_CURVE ( 'NONE', #16174, #17311, #10874, .T. ) ;
#3045 = EDGE_CURVE ( 'NONE', #9189, #8319, #3244, .T. ) ;
#3046 = CARTESIAN_POINT ( 'NONE',  ( 16.56753206892534891, -0.008490833999798035742, 0.004253784598196731770 ) ) ;
#3047 = ORIENTED_EDGE ( 'NONE', *, *, #13523, .F. ) ;
#3048 = CARTESIAN_POINT ( 'NONE',  ( -0.2192422490275049152, -45.00000000000000000, 6.000000000000000000 ) ) ;
#3049 = UNCERTAINTY_MEASURE_WITH_UNIT (LENGTH_MEASURE( 1.000000000000000082E-05 ), #15530, 'distance_accuracy_value', 'NONE');
#3050 = CARTESIAN_POINT ( 'NONE',  ( 6.279379834064825694, -3.098285787162885718, -12.00000000061317884 ) ) ;
#3051 = ORIENTED_EDGE ( 'NONE', *, *, #7216, .F. ) ;
#3052 = CARTESIAN_POINT ( 'NONE',  ( 2.353870697619111496, 8.216087327473076130, -10.00946331859655203 ) ) ;
#3053 = CARTESIAN_POINT ( 'NONE',  ( 15.00000000000000711, -24.99999999999999645, 6.000000000000000000 ) ) ;
#3054 = CARTESIAN_POINT ( 'NONE',  ( 8.522092701127531811, -1.786985377231985694, -6.722964936702116034 ) ) ;
#3055 = CARTESIAN_POINT ( 'NONE',  ( 20.00000000000000711, -40.00000000000000000, 6.000000000000000000 ) ) ;
#3056 = B_SPLINE_CURVE_WITH_KNOTS ( 'NONE', 3,
 ( #3335, #386, #4883, #4781 ),
 .UNSPECIFIED., .F., .F.,
 ( 4, 4 ),
 ( 1.629624753548408703E-17, 0.003005512676784843126 ),
 .UNSPECIFIED. ) ;
#3057 = ORIENTED_EDGE ( 'NONE', *, *, #15897, .F. ) ;
#3058 = PRESENTATION_STYLE_ASSIGNMENT (( #4615 ) ) ;
#3059 = DIRECTION ( 'NONE',  ( 0.000000000000000000, 0.000000000000000000, 1.000000000000000000 ) ) ;
#3060 = CARTESIAN_POINT ( 'NONE',  ( 16.58200780006414732, 0.006043560077721710048, -0.009393638146078546122 ) ) ;
#3061 = CARTESIAN_POINT ( 'NONE',  ( 3.950837973638668288, 0.000000000000000000, 0.000000000000000000 ) ) ;
#3062 = CARTESIAN_POINT ( 'NONE',  ( 2.353870697619109720, 10.90705766126230536, -6.980654702310723714 ) ) ;
#3063 = CARTESIAN_POINT ( 'NONE',  ( 3.074695600508088322, 15.41438262616131283, 2.093687500611883578 ) ) ;
#3064 = ORIENTED_EDGE ( 'NONE', *, *, #7041, .F. ) ;
#3065 = CARTESIAN_POINT ( 'NONE',  ( 0.3137051932979792457, -8.442169467526928983, 10.83767969834800127 ) ) ;
#3066 = CARTESIAN_POINT ( 'NONE',  ( 0.4862570985993235340, -8.769551628660655851, -10.79774104611382946 ) ) ;
#3067 = ORIENTED_EDGE ( 'NONE', *, *, #221, .T. ) ;
#3068 = ORIENTED_EDGE ( 'NONE', *, *, #16880, .T. ) ;
#3070 = DIRECTION ( 'NONE',  ( 0.000000000000000000, 0.000000000000000000, -1.000000000000000000 ) ) ;
#3069 = VECTOR ( 'NONE', #7854, 1000.000000000000000 ) ;
#3071 = EDGE_CURVE ( 'NONE', #14584, #13704, #17452, .T. ) ;
#3072 = ORIENTED_EDGE ( 'NONE', *, *, #9354, .T. ) ;
#3073 = CARTESIAN_POINT ( 'NONE',  ( -2.179449471770337432, -4.500000000000000000, 0.000000000000000000 ) ) ;
#3074 = EDGE_LOOP ( 'NONE', ( #17384, #8165, #2527, #2937 ) ) ;
#3075 = CARTESIAN_POINT ( 'NONE',  ( 16.56782317627811096, 0.002708056627497615852, -0.009439921864426480472 ) ) ;
#3076 = SURFACE_STYLE_USAGE ( .BOTH. , #10364 ) ;
#3077 = FACE_OUTER_BOUND ( 'NONE', #13363, .T. ) ;
#3078 =( BOUNDED_SURFACE ( )  B_SPLINE_SURFACE ( 3, 1, ( 
 ( #7423, #17835 ),
 ( #7328, #1675 ),
 ( #13141, #51 ),
 ( #2993, #13234 ) ),
 .UNSPECIFIED., .F., .F., .T. ) 
 B_SPLINE_SURFACE_WITH_KNOTS ( ( 4, 4 ),
 ( 2, 2 ),
 ( 0.000000000000000000, 1.000000000000000000 ),
 ( 0.000000000000000000, 1.000000000000000000 ),
 .UNSPECIFIED. ) 
 GEOMETRIC_REPRESENTATION_ITEM ( )  RATIONAL_B_SPLINE_SURFACE ( (
 ( 1.000000000000000000, 1.000000000000000000),
 ( 0.7792777138730160313, 0.9689936506012927220),
 ( 0.7792777138730160313, 0.9689936506012927220),
 ( 1.000000000000000000, 1.000000000000000000) ) ) 
 REPRESENTATION_ITEM ( '' )  SURFACE ( )  );
#3079 = CARTESIAN_POINT ( 'NONE',  ( 1.861628059977343153, -4.358833901513129661, 11.66985327793197236 ) ) ;
#3080 = UNCERTAINTY_MEASURE_WITH_UNIT (LENGTH_MEASURE( 1.000000000000000082E-05 ), #13302, 'distance_accuracy_value', 'NONE');
#3081 = CARTESIAN_POINT ( 'NONE',  ( 3.950837973638668288, 0.000000000000000000, 0.000000000000000000 ) ) ;
#3082 = LINE ( 'NONE', #15996, #9638 ) ;
#3083 = CARTESIAN_POINT ( 'NONE',  ( 16.56872352241294521, 0.007240717549633888563, 0.007512283835804339609 ) ) ;
#3084 = LINE ( 'NONE', #10175, #6365 ) ;
#3085 = ORIENTED_EDGE ( 'NONE', *, *, #8316, .F. ) ;
#3086 = EDGE_CURVE ( 'NONE', #9019, #4326, #3904, .T. ) ;
#3087 = CARTESIAN_POINT ( 'NONE',  ( -33.49999999999999289, -12.50000000000000178, -0.5000000000000000000 ) ) ;
#3088 = CARTESIAN_POINT ( 'NONE',  ( -30.00000000000000355, -12.50000000000000178, 6.000000000000000000 ) ) ;
#3089 = PRODUCT_DEFINITION ( 'UNKNOWN', '', #2541, #4217 ) ;
#3090 = DIRECTION ( 'NONE',  ( 0.7635533937278214944, -0.1790966170213922626, -0.6204116510013485408 ) ) ;
#3091 = VECTOR ( 'NONE', #6397, 1000.000000000000114 ) ;
#3092 = CARTESIAN_POINT ( 'NONE',  ( 2.123976203522053741, 11.67822624909940821, -10.37815841598478883 ) ) ;
#3093 = EDGE_CURVE ( 'NONE', #15469, #13788, #11771, .T. ) ;
#3094 = EDGE_LOOP ( 'NONE', ( #10283, #18034, #4, #3122 ) ) ;
#3095 = ADVANCED_FACE ( 'NONE', ( #18420 ), #15464, .T. ) ;
#3096 = ORIENTED_EDGE ( 'NONE', *, *, #8885, .F. ) ;
#3097 = ADVANCED_FACE ( 'NONE', ( #16726 ), #15371, .F. ) ;
#3098 = EDGE_LOOP ( 'NONE', ( #15137, #11889, #11163, #16800 ) ) ;
#3099 = ORIENTED_EDGE ( 'NONE', *, *, #13998, .T. ) ;
#3100 = CARTESIAN_POINT ( 'NONE',  ( 0.3137051932979775248, 0.4596302728639756197, 13.73004976592202198 ) ) ;
#3101 = FACE_BOUND ( 'NONE', #522, .T. ) ;
#3102 = FACE_OUTER_BOUND ( 'NONE', #9668, .T. ) ;
#3103 = VERTEX_POINT ( 'NONE', #939 ) ;
#3104 = DIRECTION ( 'NONE',  ( 0.000000000000000000, 0.000000000000000000, 1.000000000000000000 ) ) ;
#3105 = CARTESIAN_POINT ( 'NONE',  ( 2.636624412714236865, 0.000000000000000000, 0.000000000000000000 ) ) ;
#3106 = CYLINDRICAL_SURFACE ( 'NONE', #3645, 5.000000000000000000 ) ;
#3107 = CARTESIAN_POINT ( 'NONE',  ( 16.56782317627811096, -0.002708056627497679603, 0.009439921864426459655 ) ) ;
#3108 = VECTOR ( 'NONE', #3705, 1000.000000000000000 ) ;
#3109 = EDGE_CURVE ( 'NONE', #6836, #6081, #11271, .T. ) ;
#3110 = FACE_OUTER_BOUND ( 'NONE', #7738, .T. ) ;
#3111 = CARTESIAN_POINT ( 'NONE',  ( 0.3137051932979757485, -11.37800749014125223, -7.698472063774596030 ) ) ;
#3112 = FACE_OUTER_BOUND ( 'NONE', #14632, .T. ) ;
#3113 = ORIENTED_EDGE ( 'NONE', *, *, #14292, .T. ) ;
#3114 = EDGE_CURVE ( 'NONE', #11324, #13735, #3993, .T. ) ;
#3115 =( BOUNDED_SURFACE ( )  B_SPLINE_SURFACE ( 3, 1, ( 
 ( #12045, #12148 ),
 ( #10517, #4592 ),
 ( #7568, #13378 ),
 ( #10416, #292 ) ),
 .UNSPECIFIED., .F., .F., .T. ) 
 B_SPLINE_SURFACE_WITH_KNOTS ( ( 4, 4 ),
 ( 2, 2 ),
 ( 0.000000000000000000, 1.000000000000000000 ),
 ( 0.000000000000000000, 1.000000000000000000 ),
 .UNSPECIFIED. ) 
 GEOMETRIC_REPRESENTATION_ITEM ( )  RATIONAL_B_SPLINE_SURFACE ( (
 ( 1.000000000000000000, 1.000000000000000000),
 ( 0.7792777138730160313, 0.9689936506012927220),
 ( 0.7792777138730160313, 0.9689936506012927220),
 ( 1.000000000000000000, 1.000000000000000000) ) ) 
 REPRESENTATION_ITEM ( '' )  SURFACE ( )  );
#3116 =( BOUNDED_SURFACE ( )  B_SPLINE_SURFACE ( 3, 1, ( 
 ( #18559, #5461 ),
 ( #802, #9848 ),
 ( #18288, #15684 ),
 ( #2587, #1167 ) ),
 .UNSPECIFIED., .F., .F., .T. ) 
 B_SPLINE_SURFACE_WITH_KNOTS ( ( 4, 4 ),
 ( 2, 2 ),
 ( 0.000000000000000000, 1.000000000000000000 ),
 ( 0.000000000000000000, 1.000000000000000000 ),
 .UNSPECIFIED. ) 
 GEOMETRIC_REPRESENTATION_ITEM ( )  RATIONAL_B_SPLINE_SURFACE ( (
 ( 1.000000000000000000, 1.000000000000000000),
 ( 0.7792777138730160313, 0.9689936506012927220),
 ( 0.7792777138730160313, 0.9689936506012927220),
 ( 1.000000000000000000, 1.000000000000000000) ) ) 
 REPRESENTATION_ITEM ( '' )  SURFACE ( )  );
#3117 = VERTEX_POINT ( 'NONE', #853 ) ;
#3118 = ORIENTED_EDGE ( 'NONE', *, *, #12569, .T. ) ;
#3119 = APPLICATION_CONTEXT ( 'automotive_design' ) ;
#3120 = EDGE_LOOP ( 'NONE', ( #11267, #5072 ) ) ;
#3121 = DIRECTION ( 'NONE',  ( 0.000000000000000000, 0.000000000000000000, -1.000000000000000000 ) ) ;
#3122 = ORIENTED_EDGE ( 'NONE', *, *, #14202, .T. ) ;
#3123 = FACE_OUTER_BOUND ( 'NONE', #18092, .T. ) ;
#3124 = SPHERICAL_SURFACE ( 'NONE', #14476, 5.000000000000000000 ) ;
#3125 = CARTESIAN_POINT ( 'NONE',  ( 0.8740779401510754276, -9.070947476926809472, -11.05257166392059354 ) ) ;
#3126 = CARTESIAN_POINT ( 'NONE',  ( -4.999999999999995559, -27.00000000000000000, 31.00000000000000000 ) ) ;
#3127 = EDGE_LOOP ( 'NONE', ( #13679, #11435, #11316, #6059 ) ) ;
#3128 = CARTESIAN_POINT ( 'NONE',  ( 0.4384471787762797002, 3.577367180593735263, -13.39294437382614333 ) ) ;
#3129 = CARTESIAN_POINT ( 'NONE',  ( 0.3151928476913583022, 13.06684726503526761, 4.245457024760265874 ) ) ;
#3130 = CARTESIAN_POINT ( 'NONE',  ( -6.238556470687012911, 7.499999999999999112, -16.99999999974153297 ) ) ;
#3131 = SPHERICAL_SURFACE ( 'NONE', #5399, 5.000000000000000000 ) ;
#3132 = CARTESIAN_POINT ( 'NONE',  ( 1.977436885025100510, 3.321781585409006698, 15.04044112860174209 ) ) ;
#3133 = EDGE_CURVE ( 'NONE', #5702, #15056, #4013, .T. ) ;
#3134 = CARTESIAN_POINT ( 'NONE',  ( 0.3148213771069380829, 12.99360322443203053, 4.463459503829039221 ) ) ;
#3135 = CARTESIAN_POINT ( 'NONE',  ( 0.3095370825347224519, -8.444334731363925428, -10.84046130709067768 ) ) ;
#3136 = VERTEX_POINT ( 'NONE', #5333 ) ;
#3137 = ORIENTED_EDGE ( 'NONE', *, *, #15735, .T. ) ;
#3138 = DIRECTION ( 'NONE',  ( -0.000000000000000000, -0.000000000000000000, 1.000000000000000000 ) ) ;
#3140 = VERTEX_POINT ( 'NONE', #2452 ) ;
#3139 = LINE ( 'NONE', #1928, #16071 ) ;
#3141 = DIRECTION ( 'NONE',  ( -0.7561779333270775005, -0.4122479608995667788, -0.5081796452863290847 ) ) ;
#3142 = AXIS2_PLACEMENT_3D ( 'NONE', #18873, #11618, #4642 ) ;
#3143 = VECTOR ( 'NONE', #17164, 1000.000000000000000 ) ;
#3144 = FACE_OUTER_BOUND ( 'NONE', #15521, .T. ) ;
#3145 = VERTEX_POINT ( 'NONE', #14221 ) ;
#3146 = CARTESIAN_POINT ( 'NONE',  ( -20.00000000000000000, 2.499999999999998668, -12.00000000000000000 ) ) ;
#3147 = CARTESIAN_POINT ( 'NONE',  ( 6.344274892086337658, -2.961199469785586125, -11.99999999981462295 ) ) ;
#3148 = VERTEX_POINT ( 'NONE', #6501 ) ;
#3149 = CARTESIAN_POINT ( 'NONE',  ( -30.00000000000000711, 20.00000000000000000, 3.000000000000000000 ) ) ;
#3150 = CARTESIAN_POINT ( 'NONE',  ( 0.3137051932979792457, -0.4596302728640728752, 13.73004976592201842 ) ) ;
#3151 = CARTESIAN_POINT ( 'NONE',  ( 1.846138399168762101, 12.43476674860266584, 0.4167076046095977149 ) ) ;
#3152 = CARTESIAN_POINT ( 'NONE',  ( 0.3132635586635977298, -13.72732610560088418, 0.5277914263192632349 ) ) ;
#3153 = EDGE_CURVE ( 'NONE', #10713, #13922, #15202, .T. ) ;
#3154 = ADVANCED_FACE ( 'NONE', ( #18154 ), #16318, .F. ) ;
#3155 = EDGE_CURVE ( 'NONE', #2315, #15773, #4666, .T. ) ;
#3156 = AXIS2_PLACEMENT_3D ( 'NONE', #11084, #16899, #5053 ) ;
#3157 = VECTOR ( 'NONE', #4687, 1000.000000000000114 ) ;
#3158 = ORIENTED_EDGE ( 'NONE', *, *, #4711, .F. ) ;
#3159 = EDGE_CURVE ( 'NONE', #4745, #5087, #16034, .T. ) ;
#3160 = CARTESIAN_POINT ( 'NONE',  ( 3.512766787570714477, -14.81029789862161117, -2.682019731918549255 ) ) ;
#3161 = CARTESIAN_POINT ( 'NONE',  ( 16.57210152137263393, -0.003862718596009374894, -0.01402404281922920576 ) ) ;
#3162 = CARTESIAN_POINT ( 'NONE',  ( 16.57778382496167424, -0.006312874906843772387, 0.01354073047775764503 ) ) ;
#3163 = CARTESIAN_POINT ( 'NONE',  ( 0.3939875929385671105, 11.57636969881034084, 7.545068896001249747 ) ) ;
#3164 = CARTESIAN_POINT ( 'NONE',  ( 16.57210152137263393, 0.0006600038696347836076, 0.01453130299868640209 ) ) ;
#3165 = EDGE_LOOP ( 'NONE', ( #13969, #1526, #1502, #12720 ) ) ;
#3166 = CARTESIAN_POINT ( 'NONE',  ( 0.3150692679895994996, -4.391039771493759680, 13.01874238516608884 ) ) ;
#3167 = DIRECTION ( 'NONE',  ( 1.000000000000000000, 0.000000000000000000, 0.000000000000000000 ) ) ;
#3168 = EDGE_LOOP ( 'NONE', ( #3631, #18900, #4290, #7846 ) ) ;
#3169 = VERTEX_POINT ( 'NONE', #9908 ) ;
#3170 = CARTESIAN_POINT ( 'NONE',  ( 0.3150686449036038117, 11.02450593298030412, -8.199336701264417826 ) ) ;
#3171 = AXIS2_PLACEMENT_3D ( 'NONE', #13697, #4906, #10736 ) ;
#3172 = ORIENTED_EDGE ( 'NONE', *, *, #8065, .F. ) ;
#3173 = CARTESIAN_POINT ( 'NONE',  ( 0.4754618798421162973, 5.007009103465432709, -12.98792082933639058 ) ) ;
#3174 = EDGE_LOOP ( 'NONE', ( #4378, #7091, #14507, #18389 ) ) ;
#3175 = CARTESIAN_POINT ( 'NONE',  ( 1.846524061778019199, 10.27028962889607477, -7.023652644192158512 ) ) ;
#3176 =( NAMED_UNIT ( * ) SI_UNIT ( $, .STERADIAN. ) SOLID_ANGLE_UNIT ( ) );
#3177 = CARTESIAN_POINT ( 'NONE',  ( 3.074695600507123761, 2.093687500612191776, -15.41438262616238575 ) ) ;
#3178 = FACE_OUTER_BOUND ( 'NONE', #16382, .T. ) ;
#3179 = LINE ( 'NONE', #4545, #8102 ) ;
#3180 = FACE_OUTER_BOUND ( 'NONE', #8133, .T. ) ;
#3181 = VECTOR ( 'NONE', #11726, 1000.000000000000000 ) ;
#3182 = CARTESIAN_POINT ( 'NONE',  ( -194.9999999999999716, -5.000000000000024869, 3.000000000000000000 ) ) ;
#3183 = DIRECTION ( 'NONE',  ( -0.000000000000000000, 1.000000000000000000, -0.000000000000000000 ) ) ;
#3184 = EDGE_CURVE ( 'NONE', #12792, #17093, #7411, .T. ) ;
#3185 = VECTOR ( 'NONE', #6992, 1000.000000000000000 ) ;
#3186 = CARTESIAN_POINT ( 'NONE',  ( 16.58200780006414732, 0.01041078477703982763, -0.004047297414157931088 ) ) ;
#3187 = AXIS2_PLACEMENT_3D ( 'NONE', #18811, #1708, #7167 ) ;
#3188 = CARTESIAN_POINT ( 'NONE',  ( 0.4862570985993235340, -7.559321496869339185, -11.67702470553373750 ) ) ;
#3189 = CARTESIAN_POINT ( 'NONE',  ( 1.847412631396500693, -11.82061107079961992, -3.886120457021520647 ) ) ;
#3190 = CARTESIAN_POINT ( 'NONE',  ( 0.3170788640506440603, -13.74111462631963398, -0.1533108587037582682 ) ) ;
#3191 = VERTEX_POINT ( 'NONE', #1407 ) ;
#3192 = EDGE_CURVE ( 'NONE', #978, #9121, #613, .T. ) ;
#3193 = ORIENTED_EDGE ( 'NONE', *, *, #17742, .F. ) ;
#3194 = ORIENTED_EDGE ( 'NONE', *, *, #744, .T. ) ;
#3195 = VERTEX_POINT ( 'NONE', #1306 ) ;
#3196 =( BOUNDED_SURFACE ( )  B_SPLINE_SURFACE ( 3, 1, ( 
 ( #5197, #7488 ),
 ( #8719, #16176 ),
 ( #7203, #14641 ),
 ( #11681, #6050 ) ),
 .UNSPECIFIED., .F., .F., .T. ) 
 B_SPLINE_SURFACE_WITH_KNOTS ( ( 4, 4 ),
 ( 2, 2 ),
 ( 0.000000000000000000, 1.000000000000000000 ),
 ( 0.000000000000000000, 1.000000000000000000 ),
 .UNSPECIFIED. ) 
 GEOMETRIC_REPRESENTATION_ITEM ( )  RATIONAL_B_SPLINE_SURFACE ( (
 ( 1.000000000000000000, 1.000000000000000000),
 ( 0.9593108457356467333, 0.9995965569486454649),
 ( 0.9593108457356467333, 0.9995965569486454649),
 ( 1.000000000000000000, 1.000000000000000000) ) ) 
 REPRESENTATION_ITEM ( '' )  SURFACE ( )  );
#3197 = CARTESIAN_POINT ( 'NONE',  ( -20.00000000000000000, -2.500000000000000444, -17.00000000000000000 ) ) ;
#3198 = CARTESIAN_POINT ( 'NONE',  ( -59.99999999999997158, -10.00000000000000888, 3.000000000000000000 ) ) ;
#3199 = CONICAL_SURFACE ( 'NONE', #3536, 16.06066017081991149, 0.7853981625000062694 ) ;
#3200 = CARTESIAN_POINT ( 'NONE',  ( 1.847461586945731371, -12.44326124954594448, 0.03350899125588503030 ) ) ;
#3201 = CARTESIAN_POINT ( 'NONE',  ( 0.4862570985993235340, -3.580942890621579444, -13.44146924561384537 ) ) ;
#3202 = CARTESIAN_POINT ( 'NONE',  ( 3.950837973638676281, 12.81214529934975310, 6.888253895133341409 ) ) ;
#3203 = CARTESIAN_POINT ( 'NONE',  ( 3.950837973638668288, 0.000000000000000000, 0.000000000000000000 ) ) ;
#3204 = CARTESIAN_POINT ( 'NONE',  ( 16.58200780006414732, 0.007066318000006001528, -0.008650561019685833880 ) ) ;
#3205 = CARTESIAN_POINT ( 'NONE',  ( 1.847461586945730483, 12.44326124954594626, -0.03350899125597195383 ) ) ;
#3206 = EDGE_CURVE ( 'NONE', #11719, #17807, #17906, .T. ) ;
#3207 = CARTESIAN_POINT ( 'NONE',  ( 1.861706995891666550, -4.359009869687166194, -11.66987142852988946 ) ) ;
#3208 = DIRECTION ( 'NONE',  ( 0.000000000000000000, 0.000000000000000000, 1.000000000000000000 ) ) ;
#3209 = EDGE_CURVE ( 'NONE', #4291, #2287, #8093, .T. ) ;
#3210 = LINE ( 'NONE', #3014, #7055 ) ;
#3211 = EDGE_CURVE ( 'NONE', #11605, #8961, #1117, .T. ) ;
#3212 = CARTESIAN_POINT ( 'NONE',  ( 0.000000000000000000, 0.000000000000000000, 0.000000000000000000 ) ) ;
#3213 = CARTESIAN_POINT ( 'NONE',  ( 1.847461586945728707, 7.341074796295939286, 10.04711372545047254 ) ) ;
#3214 = EDGE_LOOP ( 'NONE', ( #4994, #3976, #1782 ) ) ;
#3215 = AXIS2_PLACEMENT_3D ( 'NONE', #3879, #828, #9981 ) ;
#3216 = EDGE_CURVE ( 'NONE', #14389, #9064, #18605, .T. ) ;
#3217 = ORIENTED_EDGE ( 'NONE', *, *, #6850, .F. ) ;
#3218 = ORIENTED_EDGE ( 'NONE', *, *, #8590, .T. ) ;
#3219 = ORIENTED_EDGE ( 'NONE', *, *, #5723, .F. ) ;
#3220 = CARTESIAN_POINT ( 'NONE',  ( 1.847372867223024961, -7.228345833872678483, -10.12831093686730100 ) ) ;
#3221 = EDGE_CURVE ( 'NONE', #16117, #12360, #17266, .T. ) ;
#3222 = DIRECTION ( 'NONE',  ( 0.000000000000000000, 0.000000000000000000, 1.000000000000000000 ) ) ;
#3223 = LINE ( 'NONE', #9070, #4117 ) ;
#3224 = CARTESIAN_POINT ( 'NONE',  ( 0.3095370825347233956, 4.681152801286161846, 12.91933430393609683 ) ) ;
#3225 = DIRECTION ( 'NONE',  ( 0.000000000000000000, -1.000000000000000000, 0.000000000000000000 ) ) ;
#3226 = ORIENTED_EDGE ( 'NONE', *, *, #6065, .F. ) ;
#3227 = CARTESIAN_POINT ( 'NONE',  ( -3.381675179273344600, 7.499999999999998224, -16.15172605159659014 ) ) ;
#3228 = CARTESIAN_POINT ( 'NONE',  ( 0.3148213771069380829, 12.99360322443203053, 4.463459503829039221 ) ) ;
#3229 = CARTESIAN_POINT ( 'NONE',  ( 2.123976203522053741, 1.531817366691752502, 15.54801196254787676 ) ) ;
#3230 = CARTESIAN_POINT ( 'NONE',  ( 0.3058872367615226295, 12.87003593440628357, 4.821066432589371509 ) ) ;
#3231 = MECHANICAL_DESIGN_GEOMETRIC_PRESENTATION_REPRESENTATION (  '', ( #9367 ), #5997 ) ;
#3232 = DIRECTION ( 'NONE',  ( -1.000000000000000000, 0.000000000000000000, 0.000000000000000000 ) ) ;
#3233 =( BOUNDED_SURFACE ( )  B_SPLINE_SURFACE ( 3, 1, ( 
 ( #7310, #17237 ),
 ( #8731, #17431 ),
 ( #7113, #17626 ),
 ( #8635, #13127 ) ),
 .UNSPECIFIED., .F., .F., .T. ) 
 B_SPLINE_SURFACE_WITH_KNOTS ( ( 4, 4 ),
 ( 2, 2 ),
 ( 0.000000000000000000, 1.000000000000000000 ),
 ( 0.000000000000000000, 1.000000000000000000 ),
 .UNSPECIFIED. ) 
 GEOMETRIC_REPRESENTATION_ITEM ( )  RATIONAL_B_SPLINE_SURFACE ( (
 ( 1.000000000000000000, 1.000000000000000000),
 ( 0.7792777138730160313, 0.9689936506012927220),
 ( 0.7792777138730160313, 0.9689936506012927220),
 ( 1.000000000000000000, 1.000000000000000000) ) ) 
 REPRESENTATION_ITEM ( '' )  SURFACE ( )  );
#3234 = DIRECTION ( 'NONE',  ( 0.000000000000000000, -1.000000000000000000, -0.000000000000000000 ) ) ;
#3235 = EDGE_LOOP ( 'NONE', ( #3338, #5545, #6726, #16756 ) ) ;
#3236 = CARTESIAN_POINT ( 'NONE',  ( 2.320520222536482713, 14.32454429810331220, 6.542539914239615229 ) ) ;
#3238 = ORIENTED_EDGE ( 'NONE', *, *, #17327, .F. ) ;
#3237 = CARTESIAN_POINT ( 'NONE',  ( 8.438534575730034959, -6.454982381540271597, -2.341351102130346362 ) ) ;
#3239 = CARTESIAN_POINT ( 'NONE',  ( 0.4862570985993252548, 11.67702470553365401, 7.559321496869467971 ) ) ;
#3240 = EDGE_CURVE ( 'NONE', #5247, #15077, #10367, .T. ) ;
#3241 = CONICAL_SURFACE ( 'NONE', #16393, 12.15840553252917289, 0.7853981625000049371 ) ;
#3242 = CARTESIAN_POINT ( 'NONE',  ( 0.3132642857406540138, -4.743831191224475496, 12.89240536501344536 ) ) ;
#3243 = AXIS2_PLACEMENT_3D ( 'NONE', #1335, #1899, #9155 ) ;
#3244 = CIRCLE ( 'NONE', #1121, 5.000000000000000888 ) ;
#3245 = ADVANCED_FACE ( 'NONE', ( #17561 ), #1820, .T. ) ;
#3246 = ORIENTED_EDGE ( 'NONE', *, *, #2566, .T. ) ;
#3247 = CARTESIAN_POINT ( 'NONE',  ( 0.3132642857406524595, -12.89240536501342760, -4.743831191224519905 ) ) ;
#3248 = PRODUCT ( 'Central Pivot', 'Central Pivot', '', ( #3764 ) ) ;
#3249 = B_SPLINE_CURVE_WITH_KNOTS ( 'NONE', 3,
 ( #5613, #17281, #14799, #4583, #17774, #16535 ),
 .UNSPECIFIED., .F., .F.,
 ( 4, 2, 4 ),
 ( 0.000000000000000000, 0.0001828790815886951050, 0.0003657581631773902100 ),
 .UNSPECIFIED. ) ;
#3250 = CARTESIAN_POINT ( 'NONE',  ( 2.166051897650331792, -7.500000000000000000, -13.14980647003173253 ) ) ;
#3251 = ORIENTED_EDGE ( 'NONE', *, *, #8948, .F. ) ;
#3252 = CARTESIAN_POINT ( 'NONE',  ( 8.438534575730034959, -1.899950616255234870, 6.598402093327873530 ) ) ;
#3253 = CARTESIAN_POINT ( 'NONE',  ( 0.3137051932979757485, 13.73004976592202020, -0.4596302728640235258 ) ) ;
#3254 = CIRCLE ( 'NONE', #13946, 5.000000000000000000 ) ;
#3255 = CARTESIAN_POINT ( 'NONE',  ( 16.57605080000000086, 0.000000000000000000, 0.000000000000000000 ) ) ;
#3256 = CARTESIAN_POINT ( 'NONE',  ( 1.977436885026283564, -11.52792723756319582, -10.21547824869606202 ) ) ;
#3257 = B_SPLINE_CURVE_WITH_KNOTS ( 'NONE', 3,
 ( #675, #12326, #17979, #5060, #16905, #487, #5245, #18156, #16548, #6317, #11090, #4885, #15288 ),
 .UNSPECIFIED., .F., .F.,
 ( 4, 3, 3, 3, 4 ),
 ( 3.035766082959412415E-18, 0.0002299780670421045197, 0.0004599561239687880061, 0.0006896788984287874130, 0.0009194956271626412558 ),
 .UNSPECIFIED. ) ;
#3258 = CIRCLE ( 'NONE', #13950, 5.000000000000000888 ) ;
#3259 = MECHANICAL_DESIGN_GEOMETRIC_PRESENTATION_REPRESENTATION (  '', ( #8169 ), #4186 ) ;
#3260 = ORIENTED_EDGE ( 'NONE', *, *, #13945, .T. ) ;
#3261 = CARTESIAN_POINT ( 'NONE',  ( 3.950837973638675393, 6.888253895133479965, -12.81214529934967672 ) ) ;
#3262 = CARTESIAN_POINT ( 'NONE',  ( 0.3150686449036065317, 11.20479228691397822, 7.951193823202440392 ) ) ;
#3263 = DIRECTION ( 'NONE',  ( 0.000000000000000000, 0.000000000000000000, -1.000000000000000000 ) ) ;
#3264 = CARTESIAN_POINT ( 'NONE',  ( 0.3095370825347224519, -7.700448427571953580, 11.38092634279625770 ) ) ;
#3265 = FACE_OUTER_BOUND ( 'NONE', #14790, .T. ) ;
#3266 = ORIENTED_EDGE ( 'NONE', *, *, #12410, .T. ) ;
#3267 = CARTESIAN_POINT ( 'NONE',  ( 0.3151930723728453843, -4.318364831037682094, 13.04315954105013198 ) ) ;
#3268 = CARTESIAN_POINT ( 'NONE',  ( -5.000000000000000888, 17.00000000000000000, 3.000000000000000000 ) ) ;
#3269 = ORIENTED_EDGE ( 'NONE', *, *, #16857, .F. ) ;
#3270 = EDGE_CURVE ( 'NONE', #8048, #14890, #5993, .T. ) ;
#3271 = EDGE_CURVE ( 'NONE', #12603, #4207, #17956, .T. ) ;
#3272 = ADVANCED_FACE ( 'NONE', ( #10488 ), #2139, .T. ) ;
#3273 = ORIENTED_EDGE ( 'NONE', *, *, #12565, .F. ) ;
#3274 = DIRECTION ( 'NONE',  ( -0.7635533937278214944, 0.3620487483322560873, -0.5347026451755899634 ) ) ;
#3275 = ORIENTED_EDGE ( 'NONE', *, *, #14937, .F. ) ;
#3276 = CARTESIAN_POINT ( 'NONE',  ( 1.861628059977344263, 3.332996951203627933, 12.00316790821102941 ) ) ;
#3277 = ORIENTED_EDGE ( 'NONE', *, *, #10758, .F. ) ;
#3278 = SURFACE_STYLE_FILL_AREA ( #1764 ) ;
#3279 = FACE_OUTER_BOUND ( 'NONE', #13417, .T. ) ;
#3280 = CARTESIAN_POINT ( 'NONE',  ( 0.3939822652208125331, -13.34132036472939831, 3.598529276937210142 ) ) ;
#3281 = AXIS2_PLACEMENT_3D ( 'NONE', #9441, #2618, #15718 ) ;
#3282 = CARTESIAN_POINT ( 'NONE',  ( 12.00000000000000711, -18.99999999999999645, 7.000000000000000000 ) ) ;
#3283 = FILL_AREA_STYLE ('',( #14663 ) ) ;
#3284 = DIRECTION ( 'NONE',  ( -1.000000000000000000, -1.239088197126290570E-16, 0.000000000000000000 ) ) ;
#3285 = B_SPLINE_CURVE_WITH_KNOTS ( 'NONE', 3,
 ( #2784, #17517, #4424, #8359, #14178, #18660, #6926, #17139, #4050, #15700, #12833, #5559, #11415 ),
 .UNSPECIFIED., .F., .F.,
 ( 4, 3, 3, 3, 4 ),
 ( 8.673617379884034509E-19, 0.0002299780670421053329, 0.0004599561239687884940, 0.0006896788984287899067, 0.0009194956271626421231 ),
 .UNSPECIFIED. ) ;
#3286 = CARTESIAN_POINT ( 'NONE',  ( 3.353306896162455253, -3.007732942432324474, -13.62210141459498303 ) ) ;
#3287 = CARTESIAN_POINT ( 'NONE',  ( -27.50000000000000711, -12.50000000000000178, 3.000000000000000000 ) ) ;
#3288 = CARTESIAN_POINT ( 'NONE',  ( 2.002547531651519996, -3.242439124566736997, 12.17374746633577232 ) ) ;
#3289 = CARTESIAN_POINT ( 'NONE',  ( 8.438534575730034959, 2.341351102130277528, 6.454982381540297354 ) ) ;
#3290 = CARTESIAN_POINT ( 'NONE',  ( 2.747332970342022840, 11.66639548242823921, -11.45495994260705075 ) ) ;
#3291 = EDGE_LOOP ( 'NONE', ( #11241, #8275, #18451, #8539 ) ) ;
#3292 = ADVANCED_FACE ( 'NONE', ( #361 ), #15681, .F. ) ;
#3293 = VECTOR ( 'NONE', #11276, 1000.000000000000000 ) ;
#3294 = EDGE_CURVE ( 'NONE', #5775, #4723, #18331, .T. ) ;
#3295 = ORIENTED_EDGE ( 'NONE', *, *, #8213, .F. ) ;
#3296 = B_SPLINE_CURVE_WITH_KNOTS ( 'NONE', 3,
 ( #13885, #12456, #15592, #14075, #12733, #3758 ),
 .UNSPECIFIED., .F., .F.,
 ( 4, 2, 4 ),
 ( 1.939479807224432123E-18, 0.001657017934711440621, 0.003314035869422879074 ),
 .UNSPECIFIED. ) ;
#3297 = ORIENTED_EDGE ( 'NONE', *, *, #3555, .F. ) ;
#3298 = ORIENTED_EDGE ( 'NONE', *, *, #8499, .F. ) ;
#3299 = B_SPLINE_CURVE_WITH_KNOTS ( 'NONE', 3,
 ( #16121, #4652, #3002, #159, #11821, #14965 ),
 .UNSPECIFIED., .F., .F.,
 ( 4, 2, 4 ),
 ( 8.940560153363745023E-19, 0.0001828790815886946442, 0.0003657581631773883669 ),
 .UNSPECIFIED. ) ;
#3300 = EDGE_CURVE ( 'NONE', #10695, #9114, #18797, .T. ) ;
#3301 = DIRECTION ( 'NONE',  ( 0.7561779333270773895, 0.2350349629540228469, -0.6106991889125047424 ) ) ;
#3302 = EDGE_CURVE ( 'NONE', #15569, #3029, #11735, .T. ) ;
#3303 = CARTESIAN_POINT ( 'NONE',  ( -27.50000000000000711, -12.50000000000000178, 6.000000000000000000 ) ) ;
#3304 = CARTESIAN_POINT ( 'NONE',  ( 1.846138399168762101, -3.446241763652916124, -11.95493567637853971 ) ) ;
#3305 = CARTESIAN_POINT ( 'NONE',  ( 22.75000000000000000, 0.000000000000000000, 2.055000000000000160 ) ) ;
#3306 = CARTESIAN_POINT ( 'NONE',  ( -194.9999999999999716, -10.00000000000002665, 3.000000000000000000 ) ) ;
#3307 = DIRECTION ( 'NONE',  ( -1.000000000000000000, -0.000000000000000000, -0.000000000000000000 ) ) ;
#3308 = CARTESIAN_POINT ( 'NONE',  ( 1.560000000000000053, 0.000000000000000000, 2.999999999999998668 ) ) ;
#3309 = DIRECTION ( 'NONE',  ( -0.000000000000000000, -0.000000000000000000, -1.000000000000000000 ) ) ;
#3310 = CARTESIAN_POINT ( 'NONE',  ( 3.686287386450715076E-15, -16.60000000000000142, 25.01316734529526187 ) ) ;
#3311 = CARTESIAN_POINT ( 'NONE',  ( 2.636624412714237309, 11.10302021257826866, 11.60464335004050973 ) ) ;
#3312 = DIRECTION ( 'NONE',  ( -1.000000000000000000, 0.000000000000000000, 0.000000000000000000 ) ) ;
#3313 = AXIS2_PLACEMENT_3D ( 'NONE', #791, #701, #15404 ) ;
#3314 = DIRECTION ( 'NONE',  ( -9.244463733058732095E-33, -1.000000000000000000, -2.533398541561207105E-17 ) ) ;
#3315 = CARTESIAN_POINT ( 'NONE',  ( 1.846138399168762101, 7.646096044339892650, 9.815003036200437236 ) ) ;
#3316 = ORIENTED_EDGE ( 'NONE', *, *, #10293, .F. ) ;
#3317 =( BOUNDED_SURFACE ( )  B_SPLINE_SURFACE ( 3, 1, ( 
 ( #14236, #8503 ),
 ( #8592, #7267 ),
 ( #1140, #12982 ),
 ( #12332, #1524 ) ),
 .UNSPECIFIED., .F., .F., .T. ) 
 B_SPLINE_SURFACE_WITH_KNOTS ( ( 4, 4 ),
 ( 2, 2 ),
 ( 0.000000000000000000, 1.000000000000000000 ),
 ( 0.000000000000000000, 1.000000000000000000 ),
 .UNSPECIFIED. ) 
 GEOMETRIC_REPRESENTATION_ITEM ( )  RATIONAL_B_SPLINE_SURFACE ( (
 ( 1.000000000000000000, 1.000000000000000000),
 ( 0.9933953342250438912, 0.8357391271907739227),
 ( 0.9933953342250438912, 0.8357391271907739227),
 ( 1.000000000000000000, 1.000000000000000000) ) ) 
 REPRESENTATION_ITEM ( '' )  SURFACE ( )  );
#3318 = ORIENTED_EDGE ( 'NONE', *, *, #9650, .T. ) ;
#3319 = ORIENTED_EDGE ( 'NONE', *, *, #1073, .F. ) ;
#3320 = VERTEX_POINT ( 'NONE', #13252 ) ;
#3321 = CARTESIAN_POINT ( 'NONE',  ( 1.977228804423517117, 14.12033626431153444, -6.152949558602713864 ) ) ;
#3322 = CARTESIAN_POINT ( 'NONE',  ( -20.00000000000000000, 2.499999999999998668, -17.00000000000000000 ) ) ;
#3323 = EDGE_CURVE ( 'NONE', #8935, #16984, #15388, .T. ) ;
#3324 = CYLINDRICAL_SURFACE ( 'NONE', #1049, 2.499999999999999556 ) ;
#3325 = CARTESIAN_POINT ( 'NONE',  ( 1.254009781011991453, -9.426200207651724838, -11.25324419414228494 ) ) ;
#3326 = CIRCLE ( 'NONE', #2410, 5.000000000000000000 ) ;
#3327 = CARTESIAN_POINT ( 'NONE',  ( 3.950837973638677170, 12.81214529934985080, -6.888253895133152227 ) ) ;
#3328 = ORIENTED_EDGE ( 'NONE', *, *, #7688, .T. ) ;
#3329 = VECTOR ( 'NONE', #12064, 1000.000000000000114 ) ;
#3330 = CARTESIAN_POINT ( 'NONE',  ( 3.337222544067826480, 7.500000000000000000, -16.12749921823413146 ) ) ;
#3331 = CARTESIAN_POINT ( 'NONE',  ( 0.3142011359265332593, 13.17934269988458063, 3.879426116491735854 ) ) ;
#3332 = CARTESIAN_POINT ( 'NONE',  ( 16.57778382496167424, 0.01482878558584569718, 0.001819584982831951199 ) ) ;
#3333 = CARTESIAN_POINT ( 'NONE',  ( 16.56782317627811096, -0.009439921864426870785, 0.002708056627498742989 ) ) ;
#3334 = VECTOR ( 'NONE', #8773, 1000.000000000000000 ) ;
#3335 = CARTESIAN_POINT ( 'NONE',  ( 3.950837973638676281, 6.316429227969464932, 13.10350451991842569 ) ) ;
#3336 = CARTESIAN_POINT ( 'NONE',  ( 2.697797270744666243, -13.26309265156976558, -0.9169917281808652731 ) ) ;
#3337 = B_SPLINE_CURVE_WITH_KNOTS ( 'NONE', 3,
 ( #3761, #18379, #9587, #6736 ),
 .UNSPECIFIED., .F., .F.,
 ( 4, 4 ),
 ( 0.000000000000000000, 0.002004993803842607548 ),
 .UNSPECIFIED. ) ;
#3338 = ORIENTED_EDGE ( 'NONE', *, *, #15287, .F. ) ;
#3339 = EDGE_CURVE ( 'NONE', #18321, #5518, #1477, .T. ) ;
#3340 = CONICAL_SURFACE ( 'NONE', #8242, 14.54644660717763927, 0.8559913436420816257 ) ;
#3341 = CARTESIAN_POINT ( 'NONE',  ( 0.4862570985993252548, -12.97920246947875889, -5.003653737315625349 ) ) ;
#3343 = VERTEX_POINT ( 'NONE', #18411 ) ;
#3342 = CARTESIAN_POINT ( 'NONE',  ( 1.847168016377980670, 11.77471791462004802, -4.022276579849838996 ) ) ;
#3344 = CARTESIAN_POINT ( 'NONE',  ( 0.4385251269669978025, 12.93791070501034390, 4.978066129061732070 ) ) ;
#3345 = B_SPLINE_CURVE_WITH_KNOTS ( 'NONE', 3,
 ( #264, #13641, #12016, #16518, #16220, #14971 ),
 .UNSPECIFIED., .F., .F.,
 ( 4, 2, 4 ),
 ( 5.421010862427522170E-19, 0.0001825746017570591031, 0.0003651492035141176641 ),
 .UNSPECIFIED. ) ;
#3346 = CARTESIAN_POINT ( 'NONE',  ( 16.56753206892534891, -0.001421777558676017277, 0.009389754735542238384 ) ) ;
#3347 = ORIENTED_EDGE ( 'NONE', *, *, #15375, .F. ) ;
#3348 = CARTESIAN_POINT ( 'NONE',  ( 16.56679352167444819, 0.008252760440870499439, 0.004277682826582289259 ) ) ;
#3349 = CARTESIAN_POINT ( 'NONE',  ( -1.329448181772147075, -7.499999999999999112, -13.08538760542149326 ) ) ;
#3350 = ORIENTED_EDGE ( 'NONE', *, *, #17148, .T. ) ;
#3351 = CARTESIAN_POINT ( 'NONE',  ( 0.4862570985993252548, -5.003653737315580052, 12.97920246947877665 ) ) ;
#3352 = CARTESIAN_POINT ( 'NONE',  ( 1.342453679581834924, -14.76648944001038544, -0.9602753779832271519 ) ) ;
#3353 = CARTESIAN_POINT ( 'NONE',  ( 0.3170788640506440603, 11.02668139258442359, 8.200855617524574370 ) ) ;
#3354 =( BOUNDED_SURFACE ( )  B_SPLINE_SURFACE ( 3, 1, ( 
 ( #17688, #16448 ),
 ( #16627, #16543 ),
 ( #3428, #4776 ),
 ( #1618, #10707 ) ),
 .UNSPECIFIED., .F., .F., .T. ) 
 B_SPLINE_SURFACE_WITH_KNOTS ( ( 4, 4 ),
 ( 2, 2 ),
 ( 0.000000000000000000, 1.000000000000000000 ),
 ( 0.000000000000000000, 1.000000000000000000 ),
 .UNSPECIFIED. ) 
 GEOMETRIC_REPRESENTATION_ITEM ( )  RATIONAL_B_SPLINE_SURFACE ( (
 ( 1.000000000000000000, 1.000000000000000000),
 ( 0.9933953342250436691, 0.8357391271907733676),
 ( 0.9933953342250436691, 0.8357391271907733676),
 ( 1.000000000000000000, 1.000000000000000000) ) ) 
 REPRESENTATION_ITEM ( '' )  SURFACE ( )  );
#3355 = CARTESIAN_POINT ( 'NONE',  ( -194.9999999999999716, 14.99999999999997513, -153.7432847437423789 ) ) ;
#3356 = ADVANCED_FACE ( 'NONE', ( #15361 ), #8378, .F. ) ;
#3357 = ORIENTED_EDGE ( 'NONE', *, *, #11407, .T. ) ;
#3358 = FILL_AREA_STYLE ('',( #5079 ) ) ;
#3359 = CARTESIAN_POINT ( 'NONE',  ( 1.846822687350018644, -10.23524390843944687, 7.075150813727085541 ) ) ;
#3360 = DIRECTION ( 'NONE',  ( 0.000000000000000000, 0.000000000000000000, 1.000000000000000000 ) ) ;
#3361 = DIRECTION ( 'NONE',  ( -1.000000000000000000, 0.000000000000000000, 0.000000000000000000 ) ) ;
#3363 = ORIENTED_EDGE ( 'NONE', *, *, #2609, .F. ) ;
#3362 = CARTESIAN_POINT ( 'NONE',  ( -27.32408120756002035, 15.00000000000000000, 3.000000000000000000 ) ) ;
#3364 = DIRECTION ( 'NONE',  ( -1.000000000000000000, 0.000000000000000000, 0.000000000000000000 ) ) ;
#3365 = ADVANCED_FACE ( 'NONE', ( #13930 ), #17655, .F. ) ;
#3366 = VERTEX_POINT ( 'NONE', #8296 ) ;
#3367 = CARTESIAN_POINT ( 'NONE',  ( 0.3150692679895986670, -8.199139630396084399, 11.02465386701225469 ) ) ;
#3368 = DIRECTION ( 'NONE',  ( 2.891205793294679312E-16, -1.000000000000000000, 0.000000000000000000 ) ) ;
#3369 = ORIENTED_EDGE ( 'NONE', *, *, #14505, .F. ) ;
#3370 = EDGE_LOOP ( 'NONE', ( #13830, #15289, #2956 ) ) ;
#3371 = DIRECTION ( 'NONE',  ( 0.000000000000000000, 0.000000000000000000, 1.000000000000000000 ) ) ;
#3372 = ORIENTED_EDGE ( 'NONE', *, *, #13975, .F. ) ;
#3373 = CARTESIAN_POINT ( 'NONE',  ( 3.664313757352976264, -7.012524439851403280, -12.42002390572634418 ) ) ;
#3374 = ORIENTED_EDGE ( 'NONE', *, *, #8392, .F. ) ;
#3375 = CARTESIAN_POINT ( 'NONE',  ( 16.56872352241294521, 0.007240717549633888563, 0.007512283835804339609 ) ) ;
#3376 = CARTESIAN_POINT ( 'NONE',  ( 16.56822296793089322, 0.007741272030791082788, 0.006547366384935537215 ) ) ;
#3377 = CARTESIAN_POINT ( 'NONE',  ( 2.123976203522053741, 3.347755036806118856, -15.26039569100256266 ) ) ;
#3378 = CARTESIAN_POINT ( 'NONE',  ( 0.4862570985993235340, -7.559321496869506163, 11.67702470553362559 ) ) ;
#3379 = CARTESIAN_POINT ( 'NONE',  ( 4.336808689942017736E-15, 0.000000000000000000, 31.00000000000000000 ) ) ;
#3380 = CARTESIAN_POINT ( 'NONE',  ( 2.636624412714236865, 0.000000000000000000, 0.000000000000000000 ) ) ;
#3381 = ADVANCED_FACE ( 'NONE', ( #5047 ), #18269, .F. ) ;
#3382 = FILL_AREA_STYLE_COLOUR ( '', #12096 ) ;
#3383 = DIRECTION ( 'NONE',  ( 0.8571673007021134438, 0.000000000000000000, 0.5150380749100522682 ) ) ;
#3384 = EDGE_CURVE ( 'NONE', #11365, #1583, #16163, .T. ) ;
#3385 = CARTESIAN_POINT ( 'NONE',  ( 0.4862570985993235340, -3.580942890621579444, -13.44146924561384537 ) ) ;
#3386 = APPLICATION_CONTEXT ( 'automotive_design' ) ;
#3387 = CARTESIAN_POINT ( 'NONE',  ( 0.4384471787762797002, 3.577367180593735263, -13.39294437382614333 ) ) ;
#3388 = CARTESIAN_POINT ( 'NONE',  ( 0.3307726912345205772, 8.558645027434268471, 10.76786801061209964 ) ) ;
#3389 = AXIS2_PLACEMENT_3D ( 'NONE', #9370, #2114, #13759 ) ;
#3390 = FACE_OUTER_BOUND ( 'NONE', #12224, .T. ) ;
#3391 = SURFACE_STYLE_USAGE ( .BOTH. , #2242 ) ;
#3392 = EDGE_LOOP ( 'NONE', ( #11101, #17625, #2053, #7778 ) ) ;
#3393 = VERTEX_POINT ( 'NONE', #11169 ) ;
#3394 = VERTEX_POINT ( 'NONE', #4961 ) ;
#3395 = VERTEX_POINT ( 'NONE', #16621 ) ;
#3396 = B_SPLINE_CURVE_WITH_KNOTS ( 'NONE', 3,
 ( #2788, #14461, #1470, #1374, #4535, #5953 ),
 .UNSPECIFIED., .F., .F.,
 ( 4, 2, 4 ),
 ( 0.000000000000000000, 0.001656992708822367915, 0.003313985417644735830 ),
 .UNSPECIFIED. ) ;
#3397 = CARTESIAN_POINT ( 'NONE',  ( -199.9999999999999716, 4.999999999999973355, 6.000000000000000000 ) ) ;
#3398 = DIRECTION ( 'NONE',  ( 1.000000000000000000, 1.913297951445007868E-16, -0.000000000000000000 ) ) ;
#3399 = CARTESIAN_POINT ( 'NONE',  ( 1.861628059977344041, 0.5393144007391995620, -12.44564375541076551 ) ) ;
#3400 = CARTESIAN_POINT ( 'NONE',  ( 0.3095370825347234511, -7.700448427571787491, -11.38092634279637139 ) ) ;
#3401 = DIRECTION ( 'NONE',  ( 1.000000000000000000, 0.000000000000000000, 0.000000000000000000 ) ) ;
#3402 = VECTOR ( 'NONE', #3460, 1000.000000000000000 ) ;
#3403 = ORIENTED_EDGE ( 'NONE', *, *, #9073, .T. ) ;
#3404 = CARTESIAN_POINT ( 'NONE',  ( 1.861628059977341154, -12.44564375541077084, -0.5393144007391572625 ) ) ;
#3405 = CARTESIAN_POINT ( 'NONE',  ( 0.8740779401508861346, -7.708543377337782054, 12.04241618260063618 ) ) ;
#3406 = CARTESIAN_POINT ( 'NONE',  ( 0.3058872367615226295, -8.562166468153792565, 10.75034008168912791 ) ) ;
#3407 = B_SPLINE_CURVE_WITH_KNOTS ( 'NONE', 3,
 ( #18311, #5218, #917, #12568, #9881, #5574 ),
 .UNSPECIFIED., .F., .F.,
 ( 4, 2, 4 ),
 ( 2.710505431213761085E-19, 0.001657017934710631590, 0.003314035869421263179 ),
 .UNSPECIFIED. ) ;
#3408 = EDGE_CURVE ( 'NONE', #15162, #13108, #8321, .T. ) ;
#3409 = CARTESIAN_POINT ( 'NONE',  ( 0.8740764193768004731, -5.211550415969136374, 13.31469591265773289 ) ) ;
#3410 = EDGE_CURVE ( 'NONE', #17372, #16531, #14936, .T. ) ;
#3411 = CARTESIAN_POINT ( 'NONE',  ( 2.002547531651519996, -11.75462648437098601, -4.532360870844453160 ) ) ;
#3412 = EDGE_CURVE ( 'NONE', #4344, #8099, #2364, .T. ) ;
#3413 = DIRECTION ( 'NONE',  ( 0.000000000000000000, 0.000000000000000000, -1.000000000000000000 ) ) ;
#3414 = AXIS2_PLACEMENT_3D ( 'NONE', #16438, #372, #16716 ) ;
#3415 = CARTESIAN_POINT ( 'NONE',  ( 3.950837973638677170, 12.81214529934985080, -6.888253895133152227 ) ) ;
#3416 = ORIENTED_EDGE ( 'NONE', *, *, #10676, .F. ) ;
#3417 = PRODUCT_DEFINITION_SHAPE ( 'NONE', 'NONE',  #18913 ) ;
#3418 = ORIENTED_EDGE ( 'NONE', *, *, #4040, .F. ) ;
#3419 = ORIENTED_EDGE ( 'NONE', *, *, #9936, .F. ) ;
#3420 = EDGE_LOOP ( 'NONE', ( #4695, #1201, #12388, #11751 ) ) ;
#3421 = CARTESIAN_POINT ( 'NONE',  ( 1.847034903785819360, -7.126331315909195219, -10.19974412751572679 ) ) ;
#3422 = DIRECTION ( 'NONE',  ( 0.000000000000000000, 0.000000000000000000, 1.000000000000000000 ) ) ;
#3423 = LINE ( 'NONE', #13460, #18761 ) ;
#3424 = CARTESIAN_POINT ( 'NONE',  ( 16.56872352241294521, 0.004907101719994633009, -0.009207754980063766539 ) ) ;
#3425 = CARTESIAN_POINT ( 'NONE',  ( 2.636624412714292376, 11.60464335004048309, 11.10302021257707850 ) ) ;
#3426 = ORIENTED_EDGE ( 'NONE', *, *, #4017, .T. ) ;
#3427 = CARTESIAN_POINT ( 'NONE',  ( 1.847380140988739594, -3.740232970470839913, 11.86779270755357807 ) ) ;
#3428 = CARTESIAN_POINT ( 'NONE',  ( 16.56822296793089322, 0.009847136207496274760, 0.002414375228568293487 ) ) ;
#3429 = CARTESIAN_POINT ( 'NONE',  ( -2.611994420159492680, 7.499999999999999112, -15.68429332095033146 ) ) ;
#3430 = B_SPLINE_CURVE_WITH_KNOTS ( 'NONE', 3,
 ( #3484, #16771, #1872, #7995, #4836, #13620 ),
 .UNSPECIFIED., .F., .F.,
 ( 4, 2, 4 ),
 ( 0.000000000000000000, 0.001500839035891553090, 0.003001678071783106180 ),
 .UNSPECIFIED. ) ;
#3431 = FACE_OUTER_BOUND ( 'NONE', #16067, .T. ) ;
#3432 =( NAMED_UNIT ( * ) SI_UNIT ( $, .STERADIAN. ) SOLID_ANGLE_UNIT ( ) );
#3433 = CARTESIAN_POINT ( 'NONE',  ( 0.3150690434770175852, 0.1531837610935626592, -13.73846430619029313 ) ) ;
#3434 =( BOUNDED_SURFACE ( )  B_SPLINE_SURFACE ( 3, 1, ( 
 ( #5843, #3264 ),
 ( #6149, #7397 ),
 ( #7302, #13497 ),
 ( #9200, #10348 ) ),
 .UNSPECIFIED., .F., .F., .T. ) 
 B_SPLINE_SURFACE_WITH_KNOTS ( ( 4, 4 ),
 ( 2, 2 ),
 ( 0.000000000000000000, 1.000000000000000000 ),
 ( 0.000000000000000000, 1.000000000000000000 ),
 .UNSPECIFIED. ) 
 GEOMETRIC_REPRESENTATION_ITEM ( )  RATIONAL_B_SPLINE_SURFACE ( (
 ( 1.000000000000000000, 1.000000000000000000),
 ( 0.9593108457356467333, 0.9995965569486454649),
 ( 0.9593108457356467333, 0.9995965569486454649),
 ( 1.000000000000000000, 1.000000000000000000) ) ) 
 REPRESENTATION_ITEM ( '' )  SURFACE ( )  );
#3435 = ORIENTED_EDGE ( 'NONE', *, *, #5415, .T. ) ;
#3436 = EDGE_CURVE ( 'NONE', #6376, #6155, #7941, .T. ) ;
#3438 = EDGE_CURVE ( 'NONE', #14673, #9334, #16720, .T. ) ;
#3437 = CARTESIAN_POINT ( 'NONE',  ( 16.56872352241294521, 0.009382111268607367521, 0.004564908236399998868 ) ) ;
#3440 = ORIENTED_EDGE ( 'NONE', *, *, #5774, .F. ) ;
#3439 = CARTESIAN_POINT ( 'NONE',  ( 16.56679352167444819, -0.008311568981098013675, -0.004162264567718770153 ) ) ;
#3441 = CARTESIAN_POINT ( 'NONE',  ( 1.918918678667046240, 11.69059232068584819, -4.466049546133788795 ) ) ;
#3442 = CARTESIAN_POINT ( 'NONE',  ( 0.3307726912345181902, 10.76786801061219734, -8.558645027434160113 ) ) ;
#3443 = EDGE_CURVE ( 'NONE', #3, #13002, #1228, .T. ) ;
#3444 = CIRCLE ( 'NONE', #7737, 5.000000000000004441 ) ;
#3445 = ORIENTED_EDGE ( 'NONE', *, *, #11834, .F. ) ;
#3446 = CARTESIAN_POINT ( 'NONE',  ( 3.074695600507442172, 6.754521329824937581, 14.01296402267882435 ) ) ;
#3447 = CARTESIAN_POINT ( 'NONE',  ( -1.334466156054568975, -7.500000000000000888, -14.76217096505567383 ) ) ;
#3448 = EDGE_LOOP ( 'NONE', ( #6925, #17991, #9352, #2182 ) ) ;
#3449 = CARTESIAN_POINT ( 'NONE',  ( 2.636624412715137922, -6.973567714907947135, 14.46769361191283920 ) ) ;
#3450 = CARTESIAN_POINT ( 'NONE',  ( 0.3150692679895987780, 13.73846569174797061, 0.1531143455845020152 ) ) ;
#3451 = CARTESIAN_POINT ( 'NONE',  ( 2.002547531651519996, -12.17374746633575988, -3.242439124566779185 ) ) ;
#3452 = DIRECTION ( 'NONE',  ( -1.000000000000000000, 0.000000000000000000, -0.000000000000000000 ) ) ;
#3453 = ORIENTED_EDGE ( 'NONE', *, *, #16965, .T. ) ;
#3454 = EDGE_CURVE ( 'NONE', #10942, #7454, #3977, .T. ) ;
#3455 = AXIS2_PLACEMENT_3D ( 'NONE', #876, #6894, #6994 ) ;
#3456 =( NAMED_UNIT ( * ) PLANE_ANGLE_UNIT ( ) SI_UNIT ( $, .RADIAN. ) );
#3457 = LINE ( 'NONE', #13493, #16294 ) ;
#3458 = EDGE_CURVE ( 'NONE', #3017, #11719, #15822, .T. ) ;
#3459 = EDGE_CURVE ( 'NONE', #16368, #9780, #9473, .T. ) ;
#3460 = DIRECTION ( 'NONE',  ( -0.8629742774544855166, 0.5052478564545411777, -0.000000000000000000 ) ) ;
#3462 = ORIENTED_EDGE ( 'NONE', *, *, #15222, .T. ) ;
#3461 = DIRECTION ( 'NONE',  ( -1.577021341797097560E-16, 1.000000000000000000, 0.000000000000000000 ) ) ;
#3463 = CARTESIAN_POINT ( 'NONE',  ( 16.57210152137263393, 0.01136813053532160708, -0.009075239946109073599 ) ) ;
#3464 = CARTESIAN_POINT ( 'NONE',  ( 16.56872352241294521, -0.009382111268607402216, -0.004564908236399935551 ) ) ;
#3465 = CARTESIAN_POINT ( 'NONE',  ( 0.4862570985993235340, -13.89016912371016943, -0.7479633556563904939 ) ) ;
#3466 = CARTESIAN_POINT ( 'NONE',  ( 0.4862570985993235340, 7.559321496869426227, 11.67702470553367711 ) ) ;
#3467 = ORIENTED_EDGE ( 'NONE', *, *, #2969, .T. ) ;
#3468 = ORIENTED_EDGE ( 'NONE', *, *, #13628, .T. ) ;
#3469 = CARTESIAN_POINT ( 'NONE',  ( 1.560000000000000053, 0.000000000000000000, 2.999999999999998668 ) ) ;
#3470 = ORIENTED_EDGE ( 'NONE', *, *, #4315, .F. ) ;
#3471 = DIRECTION ( 'NONE',  ( 0.7561779333270775005, 0.6534392409364817578, 0.03481510524965471948 ) ) ;
#3472 = ORIENTED_EDGE ( 'NONE', *, *, #12827, .T. ) ;
#3474 = DIRECTION ( 'NONE',  ( 0.000000000000000000, 0.000000000000000000, 1.000000000000000000 ) ) ;
#3473 = CIRCLE ( 'NONE', #15071, 14.54644660717763927 ) ;
#3475 = EDGE_CURVE ( 'NONE', #8324, #15452, #10593, .T. ) ;
#3476 = LINE ( 'NONE', #13510, #15540 ) ;
#3477 = AXIS2_PLACEMENT_3D ( 'NONE', #1793, #7634, #3401 ) ;
#3478 = CARTESIAN_POINT ( 'NONE',  ( 0.3151928476913592458, -13.73922860838471749, 0.0002082997483299325046 ) ) ;
#3479 = CARTESIAN_POINT ( 'NONE',  ( 1.918921323896322750, 12.49850046818175286, 0.6349083173280601899 ) ) ;
#3480 = DIRECTION ( 'NONE',  ( 5.782411586589358625E-16, -1.000000000000000000, -0.000000000000000000 ) ) ;
#3481 = CARTESIAN_POINT ( 'NONE',  ( -59.99999999999997158, -25.00000000000000711, 3.000000000000000000 ) ) ;
#3482 = DIRECTION ( 'NONE',  ( -1.000000000000000000, -0.000000000000000000, -0.000000000000000000 ) ) ;
#3483 =( NAMED_UNIT ( * ) PLANE_ANGLE_UNIT ( ) SI_UNIT ( $, .RADIAN. ) );
#3484 = CARTESIAN_POINT ( 'NONE',  ( 2.002547531651519996, 12.57989064830759496, 0.6781519942172178350 ) ) ;
#3485 = CARTESIAN_POINT ( 'NONE',  ( 3.664313757352975376, -2.831308606787148463, -13.97913389346637025 ) ) ;
#3486 = CARTESIAN_POINT ( 'NONE',  ( 16.56872352241294521, -0.001821578298043862289, 0.01027347319884366027 ) ) ;
#3487 = CARTESIAN_POINT ( 'NONE',  ( 2.320520222537280297, -15.64520721754692190, -1.795797593768913236 ) ) ;
#3488 = VECTOR ( 'NONE', #1267, 1000.000000000000000 ) ;
#3489 = CARTESIAN_POINT ( 'NONE',  ( 1.847412631396502025, -11.84727953344286533, 3.804043368582616935 ) ) ;
#3490 = CARTESIAN_POINT ( 'NONE',  ( 8.522092701127531811, 6.722964936702122252, -1.786985377231962380 ) ) ;
#3491 = CARTESIAN_POINT ( 'NONE',  ( 1.847372867223028070, 11.80112642014554325, 3.945260592619082907 ) ) ;
#3492 = ORIENTED_EDGE ( 'NONE', *, *, #14232, .T. ) ;
#3493 = ORIENTED_EDGE ( 'NONE', *, *, #11591, .F. ) ;
#3494 = VERTEX_POINT ( 'NONE', #3984 ) ;
#3495 = EDGE_LOOP ( 'NONE', ( #9973, #17749 ) ) ;
#3496 = ORIENTED_EDGE ( 'NONE', *, *, #16309, .T. ) ;
#3497 = ADVANCED_FACE ( 'NONE', ( #12680 ), #14349, .F. ) ;
#3498 = B_SPLINE_CURVE_WITH_KNOTS ( 'NONE', 3,
 ( #18810, #14511, #17101, #4203, #15384, #14604 ),
 .UNSPECIFIED., .F., .F.,
 ( 4, 2, 4 ),
 ( 0.000000000000000000, 0.001500839035891551572, 0.003001678071783103145 ),
 .UNSPECIFIED. ) ;
#3499 = B_SPLINE_CURVE_WITH_KNOTS ( 'NONE', 3,
 ( #6104, #6296, #11927, #7352, #17765, #4668, #9060, #13452, #9156, #366, #6193, #17470, #12027 ),
 .UNSPECIFIED., .F., .F.,
 ( 4, 3, 3, 3, 4 ),
 ( 4.670885906470169154E-18, 0.0002299780670421063087, 0.0004599561239687901203, 0.0006896788984287873046, 0.0009194956271626388705 ),
 .UNSPECIFIED. ) ;
#3500 = CARTESIAN_POINT ( 'NONE',  ( 1.861706995891668326, -7.751853334747247359, -9.751699138048525839 ) ) ;
#3501 = CARTESIAN_POINT ( 'NONE',  ( 2.611515231136700699, -7.500000000000001776, -15.68397129924701439 ) ) ;
#3502 = CARTESIAN_POINT ( 'NONE',  ( 0.3137051932979757485, 8.442169467526850823, 10.83767969834806166 ) ) ;
#3503 = PRODUCT_DEFINITION_CONTEXT ( 'detailed design', #7680, 'design' ) ;
#3504 = CARTESIAN_POINT ( 'NONE',  ( 2.002547531651519996, -3.242439124566566910, -12.17374746633581495 ) ) ;
#3505 = DIRECTION ( 'NONE',  ( 0.7635533937278214944, 0.5347026451755962917, -0.3620487483322465949 ) ) ;
#3506 = AXIS2_PLACEMENT_3D ( 'NONE', #12271, #6728, #18193 ) ;
#3507 = DIRECTION ( 'NONE',  ( 0.7635533937278216055, -0.5347026451755990673, 0.3620487483322425981 ) ) ;
#3508 = LINE ( 'NONE', #9346, #12008 ) ;
#3509 = CARTESIAN_POINT ( 'NONE',  ( 3.950837973638668288, 0.000000000000000000, 0.000000000000000000 ) ) ;
#3510 = B_SPLINE_CURVE_WITH_KNOTS ( 'NONE', 3,
 ( #8325, #687, #13861, #8235, #18352, #6520 ),
 .UNSPECIFIED., .F., .F.,
 ( 4, 2, 4 ),
 ( 0.000000000000000000, 0.001500839035891550705, 0.003001678071783101410 ),
 .UNSPECIFIED. ) ;
#3511 = CARTESIAN_POINT ( 'NONE',  ( 1.846138399168762989, 4.238866729160403857, 11.69739621335923729 ) ) ;
#3512 = VERTEX_POINT ( 'NONE', #1568 ) ;
#3513 = EDGE_LOOP ( 'NONE', ( #16153, #14510, #9894, #11746 ) ) ;
#3514 = EDGE_LOOP ( 'NONE', ( #13591, #4843, #18601, #1880 ) ) ;
#3515 = VECTOR ( 'NONE', #603, 1000.000000000000114 ) ;
#3516 = ORIENTED_EDGE ( 'NONE', *, *, #13944, .F. ) ;
#3517 = CIRCLE ( 'NONE', #9325, 1.000000000000000000 ) ;
#3518 = CARTESIAN_POINT ( 'NONE',  ( 1.847412631396502913, -7.278870946904175909, -10.09191835241971269 ) ) ;
#3519 = AXIS2_PLACEMENT_3D ( 'NONE', #13638, #17846, #9145 ) ;
#3520 = ADVANCED_FACE ( 'NONE', ( #17526 ), #1178, .F. ) ;
#3521 = ADVANCED_FACE ( 'NONE', ( #237 ), #11349, .T. ) ;
#3522 = EDGE_CURVE ( 'NONE', #6750, #1448, #11799, .T. ) ;
#3523 = FACE_OUTER_BOUND ( 'NONE', #5826, .T. ) ;
#3524 = CARTESIAN_POINT ( 'NONE',  ( 0.000000000000000000, -0.8660254037844384856, 1.500000000000000000 ) ) ;
#3525 = DIRECTION ( 'NONE',  ( -0.000000000000000000, 1.000000000000000000, -0.000000000000000000 ) ) ;
#3526 = CARTESIAN_POINT ( 'NONE',  ( 3.512766787570756222, -14.81029789862160762, 2.682019731918325878 ) ) ;
#3527 = ORIENTED_EDGE ( 'NONE', *, *, #15997, .T. ) ;
#3528 = CARTESIAN_POINT ( 'NONE',  ( 1.918921323896325193, -0.6349083173281016013, 12.49850046818174043 ) ) ;
#3529 = CARTESIAN_POINT ( 'NONE',  ( 2.636624412715138366, -15.91454522070249311, -2.161493821597819665 ) ) ;
#3530 = CARTESIAN_POINT ( 'NONE',  ( -6.021941181548490007, 3.575661417669479647, -12.00000000127642430 ) ) ;
#3531 = DIRECTION ( 'NONE',  ( -1.000000000000000000, 0.000000000000000000, 0.000000000000000000 ) ) ;
#3532 = CYLINDRICAL_SURFACE ( 'NONE', #9933, 5.000000000000000888 ) ;
#3533 = CARTESIAN_POINT ( 'NONE',  ( 1.342453679581834924, 13.74702459364884533, 5.476372339890065000 ) ) ;
#3534 = CARTESIAN_POINT ( 'NONE',  ( 2.705023505549866591, -8.489131503859701056, -10.24007717649589821 ) ) ;
#3535 = VECTOR ( 'NONE', #17026, 1000.000000000000000 ) ;
#3536 = AXIS2_PLACEMENT_3D ( 'NONE', #17761, #2915, #16428 ) ;
#3537 = EDGE_CURVE ( 'NONE', #18407, #9529, #14631, .T. ) ;
#3538 = VERTEX_POINT ( 'NONE', #16671 ) ;
#3540 = VERTEX_POINT ( 'NONE', #1961 ) ;
#3539 = CARTESIAN_POINT ( 'NONE',  ( 16.56753206892534891, -0.009389754735542257466, -0.001421777558675915579 ) ) ;
#3541 = DIRECTION ( 'NONE',  ( 0.000000000000000000, -0.5000000000000003331, 0.8660254037844383745 ) ) ;
#3542 = VERTEX_POINT ( 'NONE', #710 ) ;
#3543 = FACE_OUTER_BOUND ( 'NONE', #17305, .T. ) ;
#3544 = CIRCLE ( 'NONE', #7836, 3.999999999999993339 ) ;
#3545 = CARTESIAN_POINT ( 'NONE',  ( 0.5390158121842351102, -6.982261029182121881, -11.99999999709518583 ) ) ;
#3546 = EDGE_LOOP ( 'NONE', ( #17706, #13999, #7238, #5022 ) ) ;
#3547 = CARTESIAN_POINT ( 'NONE',  ( 3.353306896162453477, 9.252610477110421172, -10.44017738170046528 ) ) ;
#3548 = VECTOR ( 'NONE', #706, 1000.000000000000000 ) ;
#3549 = LINE ( 'NONE', #7874, #9457 ) ;
#3550 = EDGE_CURVE ( 'NONE', #14483, #11305, #531, .T. ) ;
#3551 = CARTESIAN_POINT ( 'NONE',  ( 0.4384471787762813100, -8.732395932355604629, -10.76632603192796722 ) ) ;
#3552 = CARTESIAN_POINT ( 'NONE',  ( 1.254255976357310010, 14.64488542023430817, 1.011593778944276822 ) ) ;
#3553 = MANIFOLD_SOLID_BREP ( 'AdvancedHole1', #9975 ) ;
#3554 = B_SPLINE_CURVE_WITH_KNOTS ( 'NONE', 3,
 ( #15575, #11107, #10756, #2476, #13514, #14141 ),
 .UNSPECIFIED., .F., .F.,
 ( 4, 2, 4 ),
 ( 3.499941646806256644E-17, 0.0001825746017570582086, 0.0003651492035140814518 ),
 .UNSPECIFIED. ) ;
#3555 = EDGE_CURVE ( 'NONE', #12470, #14610, #3476, .T. ) ;
#3556 = CARTESIAN_POINT ( 'NONE',  ( -59.99999999999997158, -25.00000000000000711, 3.000000000000000000 ) ) ;
#3557 = DIRECTION ( 'NONE',  ( 0.000000000000000000, -1.000000000000000000, 0.000000000000000000 ) ) ;
#3559 = ORIENTED_EDGE ( 'NONE', *, *, #510, .F. ) ;
#3558 = FACE_OUTER_BOUND ( 'NONE', #13481, .T. ) ;
#3560 = CARTESIAN_POINT ( 'NONE',  ( 0.3170788640506440603, 4.392045232375992647, -13.02120094575823472 ) ) ;
#3561 = DIRECTION ( 'NONE',  ( 0.7071067818211348444, 0.000000000000000000, -0.7071067805519601901 ) ) ;
#3562 = CARTESIAN_POINT ( 'NONE',  ( 3.664313757352975376, -14.16986885736091395, -1.627055439596424513 ) ) ;
#3563 = VERTEX_POINT ( 'NONE', #6162 ) ;
#3564 = ORIENTED_EDGE ( 'NONE', *, *, #11134, .F. ) ;
#3565 = DIRECTION ( 'NONE',  ( 0.000000000000000000, 0.000000000000000000, 1.000000000000000000 ) ) ;
#3566 = CIRCLE ( 'NONE', #14248, 4.750000000000000000 ) ;
#3567 = FACE_OUTER_BOUND ( 'NONE', #6810, .T. ) ;
#3568 = VERTEX_POINT ( 'NONE', #10850 ) ;
#3569 = VECTOR ( 'NONE', #7621, 1000.000000000000000 ) ;
#3570 = CARTESIAN_POINT ( 'NONE',  ( 3.950837973638675393, -14.31366178983251380, -2.591948120961955926 ) ) ;
#3571 = CONICAL_SURFACE ( 'NONE', #12123, 14.54644660717763927, 0.8559913436420816257 ) ;
#3572 = FILL_AREA_STYLE_COLOUR ( '', #16481 ) ;
#3573 = FILL_AREA_STYLE ('',( #10851 ) ) ;
#3574 = MECHANICAL_DESIGN_GEOMETRIC_PRESENTATION_REPRESENTATION (  '', ( #9380 ), #4792 ) ;
#3575 = CARTESIAN_POINT ( 'NONE',  ( 2.002547531651519996, 12.57989064830759496, 0.6781519942172178350 ) ) ;
#3576 = VECTOR ( 'NONE', #1452, 1000.000000000000000 ) ;
#3577 = PRODUCT ( 'cutting support', 'cutting support', '', ( #15240 ) ) ;
#3578 = DIRECTION ( 'NONE',  ( 0.000000000000000000, 0.000000000000000000, 1.000000000000000000 ) ) ;
#3579 = APPLICATION_PROTOCOL_DEFINITION ( 'draft international standard', 'automotive_design', 1998, #9607 ) ;
#3580 = EDGE_CURVE ( 'NONE', #10871, #8470, #9311, .T. ) ;
#3581 =( NAMED_UNIT ( * ) PLANE_ANGLE_UNIT ( ) SI_UNIT ( $, .RADIAN. ) );
#3582 = DIRECTION ( 'NONE',  ( -0.9034263296138832500, 0.000000000000000000, -0.4287433579198481337 ) ) ;
#3583 = CARTESIAN_POINT ( 'NONE',  ( 0.3939822652208109788, 0.7002900021919884477, -13.80035637018651684 ) ) ;
#3584 = VECTOR ( 'NONE', #18387, 1000.000000000000000 ) ;
#3585 = DIRECTION ( 'NONE',  ( 0.000000000000000000, 0.000000000000000000, 1.000000000000000000 ) ) ;
#3586 = CIRCLE ( 'NONE', #14264, 5.000000000000049738 ) ;
#3587 = CARTESIAN_POINT ( 'NONE',  ( 0.3939875929385636688, 8.678227324501120776, 10.75308190953746212 ) ) ;
#3588 = EDGE_CURVE ( 'NONE', #16388, #17458, #12871, .T. ) ;
#3589 = MANIFOLD_SOLID_BREP ( 'Extrude-Thin1', #12430 ) ;
#3590 = CARTESIAN_POINT ( 'NONE',  ( 0.3132635586635980074, -13.21855946425834283, -3.740017578711901436 ) ) ;
#3591 = FACE_OUTER_BOUND ( 'NONE', #730, .T. ) ;
#3592 = ORIENTED_EDGE ( 'NONE', *, *, #3109, .F. ) ;
#3593 = EDGE_LOOP ( 'NONE', ( #1132, #1706, #15924, #16239 ) ) ;
#3594 = EDGE_LOOP ( 'NONE', ( #1084, #6237, #8896, #16235, #12973 ) ) ;
#3595 = VERTEX_POINT ( 'NONE', #16395 ) ;
#3596 = VERTEX_POINT ( 'NONE', #6257 ) ;
#3597 = AXIS2_PLACEMENT_3D ( 'NONE', #17049, #8177, #902 ) ;
#3598 = CARTESIAN_POINT ( 'NONE',  ( 0.4862570985993235340, 0.7479633556562450547, 13.89016912371017831 ) ) ;
#3599 = LINE ( 'NONE', #9435, #7790 ) ;
#3600 = ORIENTED_EDGE ( 'NONE', *, *, #15222, .F. ) ;
#3601 = DIRECTION ( 'NONE',  ( -1.000000000000000000, 0.000000000000000000, 0.000000000000000000 ) ) ;
#3602 = CARTESIAN_POINT ( 'NONE',  ( 1.846613052777650976, -11.72395935470501627, 4.166957398589803852 ) ) ;
#3603 = EDGE_CURVE ( 'NONE', #10015, #2805, #7629, .T. ) ;
#3604 = PLANE ( 'NONE',  #2892 ) ;
#3605 = CARTESIAN_POINT ( 'NONE',  ( 16.56782317627811096, -0.009814734722106369796, 0.0003415813796014346851 ) ) ;
#3606 = CYLINDRICAL_SURFACE ( 'NONE', #3281, 5.000000000000000888 ) ;
#3607 = CARTESIAN_POINT ( 'NONE',  ( 0.3170788640506441158, -8.200855617524453578, -11.02668139258451063 ) ) ;
#3608 = CARTESIAN_POINT ( 'NONE',  ( 4.000000000000000000, 17.00000000000000000, 8.000000000000000000 ) ) ;
#3609 = VECTOR ( 'NONE', #4223, 1000.000000000000114 ) ;
#3610 = ADVANCED_FACE ( 'NONE', ( #4829 ), #10966, .F. ) ;
#3611 = ORIENTED_EDGE ( 'NONE', *, *, #1479, .F. ) ;
#3612 = ORIENTED_EDGE ( 'NONE', *, *, #8033, .F. ) ;
#3613 = ORIENTED_EDGE ( 'NONE', *, *, #13490, .T. ) ;
#3614 = EDGE_LOOP ( 'NONE', ( #10398, #2183, #12262, #11327 ) ) ;
#3615 = DIRECTION ( 'NONE',  ( 0.000000000000000000, -0.000000000000000000, 1.000000000000000000 ) ) ;
#3616 = CIRCLE ( 'NONE', #6058, 5.000000000000000000 ) ;
#3617 = CARTESIAN_POINT ( 'NONE',  ( 16.57210152137263393, 0.005118120558001911478, 0.01361613799508963087 ) ) ;
#3618 = CARTESIAN_POINT ( 'NONE',  ( 1.560000000000000053, -1.732050807568877859, -1.752539433813135784E-17 ) ) ;
#3619 = MANIFOLD_SOLID_BREP ( 'Fillet1', #1747 ) ;
#3620 = CARTESIAN_POINT ( 'NONE',  ( 4.000000000000000000, 20.00000000000000000, 8.000000000000000000 ) ) ;
#3621 = DIRECTION ( 'NONE',  ( 0.000000000000000000, 0.000000000000000000, 1.000000000000000000 ) ) ;
#3622 = ORIENTED_EDGE ( 'NONE', *, *, #11001, .T. ) ;
#3623 = CARTESIAN_POINT ( 'NONE',  ( 16.56822296793089322, -0.0007467251401289379167, 0.01011126603341003759 ) ) ;
#3624 = CARTESIAN_POINT ( 'NONE',  ( 2.747332970342022840, -16.12459247543628393, 2.705255688517782975 ) ) ;
#3625 = CARTESIAN_POINT ( 'NONE',  ( -4.576598828870857005, 7.499999999999742428, -13.14213029402346500 ) ) ;
#3626 = DIRECTION ( 'NONE',  ( 1.000000000000000000, 0.000000000000000000, 0.000000000000000000 ) ) ;
#3627 = FACE_OUTER_BOUND ( 'NONE', #18651, .T. ) ;
#3628 = SURFACE_STYLE_FILL_AREA ( #16729 ) ;
#3629 = DIRECTION ( 'NONE',  ( 0.000000000000000000, 0.000000000000000000, 1.000000000000000000 ) ) ;
#3630 = EDGE_CURVE ( 'NONE', #13002, #14893, #5793, .T. ) ;
#3631 = ORIENTED_EDGE ( 'NONE', *, *, #14197, .F. ) ;
#3632 = B_SPLINE_CURVE_WITH_KNOTS ( 'NONE', 3,
 ( #8619, #10148, #7296, #17042, #8347, #14164 ),
 .UNSPECIFIED., .F., .F.,
 ( 4, 2, 4 ),
 ( 4.072016404827931570E-17, 0.0002014099069817292182, 0.0004028198139634177246 ),
 .UNSPECIFIED. ) ;
#3634 = ORIENTED_EDGE ( 'NONE', *, *, #6315, .F. ) ;
#3633 = CARTESIAN_POINT ( 'NONE',  ( 1.847034903785823579, 11.90269060117939048, -3.625649561595184700 ) ) ;
#3635 = CARTESIAN_POINT ( 'NONE',  ( 1.845756295923359325, 11.97166802574126088, 3.386818134580099837 ) ) ;
#3636 = COLOUR_RGB ( '', 0.09019608, 0.27058824, 0.51372549) ;
#3637 = VERTEX_POINT ( 'NONE', #3945 ) ;
#3638 = CARTESIAN_POINT ( 'NONE',  ( 1.846613052777651198, -4.166957398589769213, -11.72395935470502870 ) ) ;
#3639 = CARTESIAN_POINT ( 'NONE',  ( -5.031681560115461416, -4.880796135282130521, -12.00000000472807926 ) ) ;
#3640 = ORIENTED_EDGE ( 'NONE', *, *, #5833, .F. ) ;
#3641 = DIRECTION ( 'NONE',  ( 0.000000000000000000, -1.734723475976806848E-16, 1.000000000000000000 ) ) ;
#3642 = CARTESIAN_POINT ( 'NONE',  ( 1.254009781011930613, -12.44229282923100932, -7.789615163754561422 ) ) ;
#3643 = CARTESIAN_POINT ( 'NONE',  ( 0.3939875929385628361, -8.678227324501040840, -10.75308190953752785 ) ) ;
#3644 = CARTESIAN_POINT ( 'NONE',  ( 1.560000000000000053, -0.8660254037844384856, 1.500000000000000000 ) ) ;
#3645 = AXIS2_PLACEMENT_3D ( 'NONE', #18041, #3601, #15345 ) ;
#3646 =( GEOMETRIC_REPRESENTATION_CONTEXT ( 3 ) GLOBAL_UNCERTAINTY_ASSIGNED_CONTEXT ( ( #4038 ) ) GLOBAL_UNIT_ASSIGNED_CONTEXT ( ( #2961, #13298, #16 ) ) REPRESENTATION_CONTEXT ( 'NONE', 'WORKASPACE' ) );
#3647 = EDGE_CURVE ( 'NONE', #10742, #3366, #4032, .T. ) ;
#3648 = EDGE_CURVE ( 'NONE', #3540, #11936, #5548, .T. ) ;
#3649 =( LENGTH_UNIT ( ) NAMED_UNIT ( * ) SI_UNIT ( .MILLI., .METRE. ) );
#3650 = CARTESIAN_POINT ( 'NONE',  ( 2.002547531651519996, -6.845637710436264456, 10.57595306287289638 ) ) ;
#3651 = EDGE_CURVE ( 'NONE', #5420, #17676, #11975, .T. ) ;
#3652 = B_SPLINE_CURVE_WITH_KNOTS ( 'NONE', 3,
 ( #765, #18339, #6240, #3812, #9548, #15376 ),
 .UNSPECIFIED., .F., .F.,
 ( 4, 2, 4 ),
 ( 1.939479807224432123E-18, 0.001500839035891553524, 0.003001678071783104879 ),
 .UNSPECIFIED. ) ;
#3653 = CARTESIAN_POINT ( 'NONE',  ( 16.56822296793089322, 0.01011126603341004106, 0.0007467251401288980180 ) ) ;
#3655 = ORIENTED_EDGE ( 'NONE', *, *, #11968, .F. ) ;
#3654 = CARTESIAN_POINT ( 'NONE',  ( 0.3939822652208131992, -11.57634296752772229, 7.545099438011985349 ) ) ;
#3656 = CARTESIAN_POINT ( 'NONE',  ( 2.002547531651519996, 7.942910686618173344, 9.778737580845726640 ) ) ;
#3657 = CARTESIAN_POINT ( 'NONE',  ( 16.56753206892534891, -0.006760771273035160941, 0.006669401563385170262 ) ) ;
#3658 = CARTESIAN_POINT ( 'NONE',  ( 3.664313757352963830, 12.97355833021539873, 5.926151963190401162 ) ) ;
#3659 = CARTESIAN_POINT ( 'NONE',  ( 1.846138399168762101, -11.69739621335925328, 4.238866729160359448 ) ) ;
#3660 = ORIENTED_EDGE ( 'NONE', *, *, #11096, .F. ) ;
#3661 = ORIENTED_EDGE ( 'NONE', *, *, #12412, .T. ) ;
#3662 = DIRECTION ( 'NONE',  ( -1.000000000000000000, -0.000000000000000000, -0.000000000000000000 ) ) ;
#3663 = CARTESIAN_POINT ( 'NONE',  ( 0.4754618798421162973, 11.68486377711966817, 7.564402563418513026 ) ) ;
#3664 = VERTEX_POINT ( 'NONE', #2408 ) ;
#3665 =( NAMED_UNIT ( * ) PLANE_ANGLE_UNIT ( ) SI_UNIT ( $, .RADIAN. ) );
#3666 = CARTESIAN_POINT ( 'NONE',  ( 0.3142011359265340920, -13.73310835363014348, 0.3830873813805846240 ) ) ;
#3667 = B_SPLINE_CURVE_WITH_KNOTS ( 'NONE', 3,
 ( #17368, #7059, #2544, #4285, #8307, #18608 ),
 .UNSPECIFIED., .F., .F.,
 ( 4, 2, 4 ),
 ( 1.748223473168675632E-18, 0.0002017457492448083403, 0.0004034914984896149459 ),
 .UNSPECIFIED. ) ;
#3668 = CARTESIAN_POINT ( 'NONE',  ( -110.4113270445337918, -81.60345299795268659, -91.28051051278382033 ) ) ;
#3669 = CARTESIAN_POINT ( 'NONE',  ( 0.3137051932979757485, -7.698472063774552510, 11.37800749014128421 ) ) ;
#3670 = CARTESIAN_POINT ( 'NONE',  ( 1.847372867223024073, 7.228345833872753978, 10.12831093686724238 ) ) ;
#3671 = PRODUCT_CONTEXT ( 'NONE', #11932, 'mechanical' ) ;
#3672 = DIRECTION ( 'NONE',  ( -1.239088197126290570E-16, 1.000000000000000000, 0.000000000000000000 ) ) ;
#3673 = CARTESIAN_POINT ( 'NONE',  ( 0.4862570985993235340, 5.003653737315670647, -12.97920246947874112 ) ) ;
#3674 = DIRECTION ( 'NONE',  ( 0.7561779333270775005, 0.03481510524965243658, -0.6534392409364818688 ) ) ;
#3675 = CIRCLE ( 'NONE', #4289, 4.000000000000000000 ) ;
#3676 = CARTESIAN_POINT ( 'NONE',  ( 2.320520222536482713, 14.32454429810331220, 6.542539914239615229 ) ) ;
#3677 = EDGE_CURVE ( 'NONE', #3979, #6216, #3296, .T. ) ;
#3678 = ADVANCED_FACE ( 'NONE', ( #6911 ), #3116, .F. ) ;
#3679 = DIRECTION ( 'NONE',  ( 1.000000000000000000, 0.000000000000000000, 0.000000000000000000 ) ) ;
#3680 = SURFACE_STYLE_FILL_AREA ( #9229 ) ;
#3681 = ORIENTED_EDGE ( 'NONE', *, *, #12726, .F. ) ;
#3682 = ORIENTED_EDGE ( 'NONE', *, *, #16814, .F. ) ;
#3683 = VERTEX_POINT ( 'NONE', #8429 ) ;
#3684 = B_SPLINE_CURVE_WITH_KNOTS ( 'NONE', 3,
 ( #212, #10341, #11873, #17712 ),
 .UNSPECIFIED., .F., .F.,
 ( 4, 4 ),
 ( 0.000000000000000000, 0.002004993803842688646 ),
 .UNSPECIFIED. ) ;
#3685 = EDGE_LOOP ( 'NONE', ( #16840, #5021, #7062, #1851 ) ) ;
#3686 = CARTESIAN_POINT ( 'NONE',  ( 0.3939875929385629472, 0.7003304234513173521, 13.80036004410494854 ) ) ;
#3687 = CARTESIAN_POINT ( 'NONE',  ( -0.1112489676725734455, -7.500000000000002665, -14.17494330110305256 ) ) ;
#3688 = ORIENTED_EDGE ( 'NONE', *, *, #2076, .F. ) ;
#3689 = CARTESIAN_POINT ( 'NONE',  ( 2.636624412714237309, 11.10302021257826866, 11.60464335004050973 ) ) ;
#3690 = CARTESIAN_POINT ( 'NONE',  ( 1.846955891736117072, -11.74973605926567188, 4.094751675596655538 ) ) ;
#3691 = CARTESIAN_POINT ( 'NONE',  ( 0.4862570985993252548, 10.79774104611373353, 8.769551628660776643 ) ) ;
#3692 = DIRECTION ( 'NONE',  ( -0.000000000000000000, -1.000000000000000000, -0.000000000000000000 ) ) ;
#3693 = AXIS2_PLACEMENT_3D ( 'NONE', #4193, #2644, #5429 ) ;
#3694 = FACE_OUTER_BOUND ( 'NONE', #2464, .T. ) ;
#3695 = ADVANCED_FACE ( 'NONE', ( #6642 ), #7005, .T. ) ;
#3696 = LINE ( 'NONE', #15350, #10169 ) ;
#3697 = LINE ( 'NONE', #568, #4485 ) ;
#3698 = ORIENTED_EDGE ( 'NONE', *, *, #8087, .T. ) ;
#3699 = ADVANCED_FACE ( 'NONE', ( #8714 ), #691, .F. ) ;
#3700 = B_SPLINE_CURVE_WITH_KNOTS ( 'NONE', 3,
 ( #13804, #7911, #5204, #9226 ),
 .UNSPECIFIED., .F., .F.,
 ( 4, 4 ),
 ( 1.226634733346699349E-18, 0.003005512676784830983 ),
 .UNSPECIFIED. ) ;
#3701 = ORIENTED_EDGE ( 'NONE', *, *, #16940, .F. ) ;
#3702 = ORIENTED_EDGE ( 'NONE', *, *, #3651, .F. ) ;
#3703 = ORIENTED_EDGE ( 'NONE', *, *, #18691, .F. ) ;
#3704 = B_SPLINE_CURVE_WITH_KNOTS ( 'NONE', 3,
 ( #13450, #363, #8862, #271 ),
 .UNSPECIFIED., .F., .F.,
 ( 4, 4 ),
 ( 0.000000000000000000, 0.002004993803842899849 ),
 .UNSPECIFIED. ) ;
#3705 = DIRECTION ( 'NONE',  ( 0.000000000000000000, 0.000000000000000000, -1.000000000000000000 ) ) ;
#3706 = VECTOR ( 'NONE', #14549, 1000.000000000000000 ) ;
#3707 = CARTESIAN_POINT ( 'NONE',  ( 0.3058872367615226295, 7.578326039752606214, 11.46514199369360298 ) ) ;
#3708 = MANIFOLD_SOLID_BREP ( 'Boss-Extrude1', #4810 ) ;
#3709 = CARTESIAN_POINT ( 'NONE',  ( 2.002547531651520885, -4.532360870844412304, 11.75462648437100377 ) ) ;
#3710 = DIRECTION ( 'NONE',  ( -0.7561779333270775005, -0.03481510524964337439, -0.6534392409364823129 ) ) ;
#3711 = VERTEX_POINT ( 'NONE', #17505 ) ;
#3712 = CARTESIAN_POINT ( 'NONE',  ( 1.847412631396505356, 10.04119192206686328, 7.348689888531877656 ) ) ;
#3713 = EDGE_CURVE ( 'NONE', #7024, #4649, #17671, .T. ) ;
#3714 = CARTESIAN_POINT ( 'NONE',  ( 2.320520222536477384, 7.743191299717406828, 13.71278186123164922 ) ) ;
#3715 = CARTESIAN_POINT ( 'NONE',  ( 0.2633197948918147846, 7.499999999999999112, -14.20553286501796997 ) ) ;
#3716 = CARTESIAN_POINT ( 'NONE',  ( 1.861628059977343819, -7.751680370225458638, 9.751736252960339968 ) ) ;
#3717 =( BOUNDED_SURFACE ( )  B_SPLINE_SURFACE ( 3, 1, ( 
 ( #15226, #517 ),
 ( #4908, #16570 ),
 ( #10738, #13699 ),
 ( #612, #6436 ) ),
 .UNSPECIFIED., .F., .F., .T. ) 
 B_SPLINE_SURFACE_WITH_KNOTS ( ( 4, 4 ),
 ( 2, 2 ),
 ( 0.000000000000000000, 1.000000000000000000 ),
 ( 0.000000000000000000, 1.000000000000000000 ),
 .UNSPECIFIED. ) 
 GEOMETRIC_REPRESENTATION_ITEM ( )  RATIONAL_B_SPLINE_SURFACE ( (
 ( 1.000000000000000000, 1.000000000000000000),
 ( 0.9933953342250436691, 0.8357391271907733676),
 ( 0.9933953342250436691, 0.8357391271907733676),
 ( 1.000000000000000000, 1.000000000000000000) ) ) 
 REPRESENTATION_ITEM ( '' )  SURFACE ( )  );
#3718 = DIRECTION ( 'NONE',  ( -0.000000000000000000, -0.000000000000000000, 1.000000000000000000 ) ) ;
#3719 = CARTESIAN_POINT ( 'NONE',  ( 3.950837973638675393, -10.05648675950118509, -10.51028938476228980 ) ) ;
#3720 = CARTESIAN_POINT ( 'NONE',  ( 0.3145729642390391323, 11.29233589755992639, 7.825496023201352180 ) ) ;
#3721 = ORIENTED_EDGE ( 'NONE', *, *, #3991, .T. ) ;
#3723 = VERTEX_POINT ( 'NONE', #10050 ) ;
#3722 = CARTESIAN_POINT ( 'NONE',  ( 2.636624412716062071, -11.10302021258080352, -11.60464335004061454 ) ) ;
#3724 = CARTESIAN_POINT ( 'NONE',  ( 3.512766787570760663, -10.87507422923897238, 10.40533104696129918 ) ) ;
#3725 = CIRCLE ( 'NONE', #54, 2.499999999999999556 ) ;
#3726 = CARTESIAN_POINT ( 'NONE',  ( 1.846524061778019199, -0.3544704288993353880, 12.43723828841088341 ) ) ;
#3727 = ADVANCED_FACE ( 'NONE', ( #5639 ), #16169, .F. ) ;
#3728 = ORIENTED_EDGE ( 'NONE', *, *, #1474, .T. ) ;
#3729 = CARTESIAN_POINT ( 'NONE',  ( 7.000000000000000000, 0.000000000000000000, 0.000000000000000000 ) ) ;
#3730 = CARTESIAN_POINT ( 'NONE',  ( -0.6549932209174553766, -7.499999999999867661, -13.04593603512842037 ) ) ;
#3731 = ORIENTED_EDGE ( 'NONE', *, *, #14047, .T. ) ;
#3732 = DIRECTION ( 'NONE',  ( -1.000000000000000000, 0.000000000000000000, 0.000000000000000000 ) ) ;
#3733 = EDGE_CURVE ( 'NONE', #13051, #13031, #6737, .T. ) ;
#3734 = CARTESIAN_POINT ( 'NONE',  ( 0.4862570985993235340, -13.44146924561383827, 3.580942890621619412 ) ) ;
#3735 = CARTESIAN_POINT ( 'NONE',  ( 2.002547531651519996, -11.75462648437098601, -4.532360870844453160 ) ) ;
#3736 = CARTESIAN_POINT ( 'NONE',  ( 1.847168016377981115, 9.955470380986737311, -7.464000291196308368 ) ) ;
#3737 = B_SPLINE_CURVE_WITH_KNOTS ( 'NONE', 3,
 ( #77, #8109, #2263, #16883 ),
 .UNSPECIFIED., .F., .F.,
 ( 4, 4 ),
 ( 0.000000000000000000, 0.002004993803842710330 ),
 .UNSPECIFIED. ) ;
#3738 = CARTESIAN_POINT ( 'NONE',  ( 0.8740779401512095426, 7.708543377337996994, -12.04241618260087776 ) ) ;
#3739 = FACE_OUTER_BOUND ( 'NONE', #6006, .T. ) ;
#3741 = ORIENTED_EDGE ( 'NONE', *, *, #4041, .T. ) ;
#3740 = FACE_BOUND ( 'NONE', #18372, .T. ) ;
#3742 = DIRECTION ( 'NONE',  ( 0.000000000000000000, -1.000000000000000000, 0.000000000000000000 ) ) ;
#3743 =( BOUNDED_SURFACE ( )  B_SPLINE_SURFACE ( 3, 1, ( 
 ( #15732, #13133 ),
 ( #9630, #1018 ),
 ( #16102, #9802 ),
 ( #2984, #14030 ) ),
 .UNSPECIFIED., .F., .F., .T. ) 
 B_SPLINE_SURFACE_WITH_KNOTS ( ( 4, 4 ),
 ( 2, 2 ),
 ( 0.000000000000000000, 1.000000000000000000 ),
 ( 0.000000000000000000, 1.000000000000000000 ),
 .UNSPECIFIED. ) 
 GEOMETRIC_REPRESENTATION_ITEM ( )  RATIONAL_B_SPLINE_SURFACE ( (
 ( 1.000000000000000000, 1.000000000000000000),
 ( 0.7792777138730160313, 0.9689936506012927220),
 ( 0.7792777138730160313, 0.9689936506012927220),
 ( 1.000000000000000000, 1.000000000000000000) ) ) 
 REPRESENTATION_ITEM ( '' )  SURFACE ( )  );
#3744 = CARTESIAN_POINT ( 'NONE',  ( 0.3058872367615226295, 3.664492643742762290, 13.24582953854926615 ) ) ;
#3745 = CARTESIAN_POINT ( 'NONE',  ( 0.3151930723728431083, -11.07033375389125673, -8.137566970826481949 ) ) ;
#3746 = CARTESIAN_POINT ( 'NONE',  ( 2.002547531651519996, -11.75462648437105173, 4.532360870844282630 ) ) ;
#3747 = ORIENTED_EDGE ( 'NONE', *, *, #8085, .T. ) ;
#3748 = ORIENTED_EDGE ( 'NONE', *, *, #3438, .F. ) ;
#3749 = CARTESIAN_POINT ( 'NONE',  ( 8.438534575730034959, -5.415535776177489602, -4.221456476902725186 ) ) ;
#3750 = APPLICATION_CONTEXT ( 'automotive_design' ) ;
#3751 = CARTESIAN_POINT ( 'NONE',  ( 16.58200780006414732, 0.006043560077721710048, -0.009393638146078546122 ) ) ;
#3752 = B_SPLINE_CURVE_WITH_KNOTS ( 'NONE', 3,
 ( #15372, #2278, #12504, #6970, #15556, #15932 ),
 .UNSPECIFIED., .F., .F.,
 ( 4, 2, 4 ),
 ( 3.897476843869763523E-18, 0.0002017457492448077711, 0.0004034914984896116391 ),
 .UNSPECIFIED. ) ;
#3753 = ORIENTED_EDGE ( 'NONE', *, *, #9599, .T. ) ;
#3754 = CARTESIAN_POINT ( 'NONE',  ( 0.3151928479966097374, 1.775918418904422640E-15, 13.73922861026898623 ) ) ;
#3755 = ADVANCED_FACE ( 'NONE', ( #1255 ), #15970, .T. ) ;
#3756 = EDGE_CURVE ( 'NONE', #12041, #8377, #13099, .T. ) ;
#3757 = EDGE_CURVE ( 'NONE', #2803, #14617, #12914, .T. ) ;
#3758 = CARTESIAN_POINT ( 'NONE',  ( 2.636624412716062960, 2.862162146982868194, -15.80357026013419564 ) ) ;
#3759 = CARTESIAN_POINT ( 'NONE',  ( 1.846138399168762101, -10.30487220521565028, -6.971848976711123136 ) ) ;
#3760 = CARTESIAN_POINT ( 'NONE',  ( -20.00000000000000000, -2.500000000000000444, -17.00000000000000000 ) ) ;
#3761 = CARTESIAN_POINT ( 'NONE',  ( 2.636624412714237309, 15.91454522070173638, -2.161493821596664144 ) ) ;
#3762 = AXIS2_PLACEMENT_3D ( 'NONE', #17444, #10467, #18870 ) ;
#3763 = CARTESIAN_POINT ( 'NONE',  ( 1.847461586945728707, 7.341074796295939286, 10.04711372545047254 ) ) ;
#3764 = PRODUCT_CONTEXT ( 'NONE', #7049, 'mechanical' ) ;
#3765 = CARTESIAN_POINT ( 'NONE',  ( 0.4754618798421162973, 0.7484603771386368898, -13.89949764182681768 ) ) ;
#3766 = CARTESIAN_POINT ( 'NONE',  ( 1.846138399168762101, -0.4167076046096411246, 12.43476674860266407 ) ) ;
#3767 = EDGE_CURVE ( 'NONE', #2949, #8066, #7293, .T. ) ;
#3768 = CARTESIAN_POINT ( 'NONE',  ( 1.846955891736117072, 7.098901504650503291, -10.21904526726839002 ) ) ;
#3769 = CARTESIAN_POINT ( 'NONE',  ( 1.977436885025421809, 14.12046670317507058, 6.153171729167918436 ) ) ;
#3770 = CARTESIAN_POINT ( 'NONE',  ( 0.4862570985993235340, -13.44146924561378498, -3.580942890621813923 ) ) ;
#3771 = CARTESIAN_POINT ( 'NONE',  ( 0.3170788640506441158, -4.100430649998053845, 13.11595226728156405 ) ) ;
#3772 = ORIENTED_EDGE ( 'NONE', *, *, #721, .T. ) ;
#3773 = AXIS2_PLACEMENT_3D ( 'NONE', #10326, #16152, #1621 ) ;
#3774 = ORIENTED_EDGE ( 'NONE', *, *, #468, .T. ) ;
#3775 = ORIENTED_EDGE ( 'NONE', *, *, #18129, .T. ) ;
#3776 = ORIENTED_EDGE ( 'NONE', *, *, #16532, .F. ) ;
#3777 = CARTESIAN_POINT ( 'NONE',  ( 0.3150692679895995552, 11.02465386701228844, 8.199139630396045320 ) ) ;
#3778 = CARTESIAN_POINT ( 'NONE',  ( 1.391363329066504617, -7.500000000000002665, -14.80343650618309503 ) ) ;
#3779 = EDGE_CURVE ( 'NONE', #1187, #11848, #7386, .T. ) ;
#3780 = LINE ( 'NONE', #14293, #17554 ) ;
#3781 = DIRECTION ( 'NONE',  ( -1.000000000000000000, 0.000000000000000000, -0.000000000000000000 ) ) ;
#3782 = FACE_OUTER_BOUND ( 'NONE', #6562, .T. ) ;
#3783 = LINE ( 'NONE', #8195, #16586 ) ;
#3784 = VECTOR ( 'NONE', #13274, 1000.000000000000000 ) ;
#3785 = CARTESIAN_POINT ( 'NONE',  ( 8.438534575730034959, 4.221456476902665678, 5.415535776177536675 ) ) ;
#3786 = AXIS2_PLACEMENT_3D ( 'NONE', #7955, #2279, #8129 ) ;
#3787 = CARTESIAN_POINT ( 'NONE',  ( 16.56753206892534891, -0.001421777558676855365, -0.009389754735541546229 ) ) ;
#3788 = CARTESIAN_POINT ( 'NONE',  ( 1.977228804422057395, -11.52787183731166820, 10.21522664410399095 ) ) ;
#3789 = CARTESIAN_POINT ( 'NONE',  ( 3.353306896162454809, 12.02594772223106645, -7.069984850384678055 ) ) ;
#3790 = ADVANCED_FACE ( 'NONE', ( #9388 ), #12895, .F. ) ;
#3791 = ORIENTED_EDGE ( 'NONE', *, *, #13250, .F. ) ;
#3792 = ORIENTED_EDGE ( 'NONE', *, *, #74, .T. ) ;
#3793 = ORIENTED_EDGE ( 'NONE', *, *, #2185, .T. ) ;
#3794 = ORIENTED_EDGE ( 'NONE', *, *, #11640, .F. ) ;
#3795 = CARTESIAN_POINT ( 'NONE',  ( 0.4754618798421171855, 8.775436892861110394, 10.80499583390516172 ) ) ;
#3796 = CARTESIAN_POINT ( 'NONE',  ( 3.950837973638675393, 14.31366178983257242, -2.591948120961654833 ) ) ;
#3797 = CARTESIAN_POINT ( 'NONE',  ( 1.342453679581834924, -13.74702459364888263, 5.476372339889963747 ) ) ;
#3798 = DIRECTION ( 'NONE',  ( 1.298018465182616140E-16, -1.000000000000000000, 0.000000000000000000 ) ) ;
#3799 = PRESENTATION_STYLE_ASSIGNMENT (( #9723 ) ) ;
#3800 = ORIENTED_EDGE ( 'NONE', *, *, #7188, .T. ) ;
#3801 = CARTESIAN_POINT ( 'NONE',  ( 0.4754618798421162973, -8.775436892861034011, -10.80499583390522567 ) ) ;
#3802 = AXIS2_PLACEMENT_3D ( 'NONE', #4204, #18711, #9924 ) ;
#3803 = CARTESIAN_POINT ( 'NONE',  ( 1.846138399168762101, -11.95493567637848109, -3.446241763653124401 ) ) ;
#3804 = EDGE_CURVE ( 'NONE', #2427, #15958, #17415, .T. ) ;
#3805 = CIRCLE ( 'NONE', #8683, 2.375000000000000444 ) ;
#3806 = CARTESIAN_POINT ( 'NONE',  ( -4.294575106066828241, 7.499999999999730882, -13.17881115347107901 ) ) ;
#3807 = CARTESIAN_POINT ( 'NONE',  ( 0.4754618798421171855, -3.583352865732766901, 13.45049478164058598 ) ) ;
#3808 = CARTESIAN_POINT ( 'NONE',  ( -66.35602477868047799, 9.999999999999973355, 5.999999999999999112 ) ) ;
#3809 = CARTESIAN_POINT ( 'NONE',  ( -205.0000000000000000, -5.000000000000024869, 6.000000000000005329 ) ) ;
#3810 = CARTESIAN_POINT ( 'NONE',  ( 2.636624412716062960, 2.862162146982868194, -15.80357026013419564 ) ) ;
#3811 = EDGE_CURVE ( 'NONE', #16337, #31, #12165, .T. ) ;
#3812 = CARTESIAN_POINT ( 'NONE',  ( 3.353306896162457029, 13.62210141459500079, -3.007732942432275181 ) ) ;
#3813 = EDGE_LOOP ( 'NONE', ( #407, #14321, #14508, #13808 ) ) ;
#3814 = CIRCLE ( 'NONE', #472, 2.500000000000000000 ) ;
#3815 = AXIS2_PLACEMENT_3D ( 'NONE', #4441, #8744, #14567 ) ;
#3817 = EDGE_LOOP ( 'NONE', ( #9700, #10501, #8493, #2511, #2931 ) ) ;
#3816 = CARTESIAN_POINT ( 'NONE',  ( -20.00000000000000000, 2.499999999999998668, -22.00000000000000000 ) ) ;
#3818 = CARTESIAN_POINT ( 'NONE',  ( 2.705023505549862595, -10.24007717649586624, 8.489131503859741912 ) ) ;
#3819 = AXIS2_PLACEMENT_3D ( 'NONE', #7749, #15092, #480 ) ;
#3820 = ADVANCED_FACE ( 'NONE', ( #11966 ), #11186, .F. ) ;
#3821 = CARTESIAN_POINT ( 'NONE',  ( 2.636624412714236865, 0.000000000000000000, 0.000000000000000000 ) ) ;
#3822 = VERTEX_POINT ( 'NONE', #12254 ) ;
#3823 = CARTESIAN_POINT ( 'NONE',  ( 2.697797270744668463, 4.970631985779762729, -12.33058466479263693 ) ) ;
#3824 = CARTESIAN_POINT ( 'NONE',  ( 1.846524061778018311, -12.43723828841088341, -0.3544704288993787422 ) ) ;
#3825 =( BOUNDED_SURFACE ( )  B_SPLINE_SURFACE ( 3, 1, ( 
 ( #50, #11905 ),
 ( #4353, #1775 ),
 ( #4449, #10275 ),
 ( #7620, #342 ) ),
 .UNSPECIFIED., .F., .F., .T. ) 
 B_SPLINE_SURFACE_WITH_KNOTS ( ( 4, 4 ),
 ( 2, 2 ),
 ( 0.000000000000000000, 1.000000000000000000 ),
 ( 0.000000000000000000, 1.000000000000000000 ),
 .UNSPECIFIED. ) 
 GEOMETRIC_REPRESENTATION_ITEM ( )  RATIONAL_B_SPLINE_SURFACE ( (
 ( 1.000000000000000000, 1.000000000000000000),
 ( 0.7792777138730158093, 0.9689936506012928330),
 ( 0.7792777138730158093, 0.9689936506012928330),
 ( 1.000000000000000000, 1.000000000000000000) ) ) 
 REPRESENTATION_ITEM ( '' )  SURFACE ( )  );
#3826 = ORIENTED_EDGE ( 'NONE', *, *, #7287, .F. ) ;
#3827 = CARTESIAN_POINT ( 'NONE',  ( -11.50000000000000178, 1.408343819019456373E-15, 10.50000000000000000 ) ) ;
#3828 = CARTESIAN_POINT ( 'NONE',  ( -4.999999999999995559, -27.00000000000000000, 6.000000000000000000 ) ) ;
#3829 = VECTOR ( 'NONE', #11704, 1000.000000000000000 ) ;
#3830 = CARTESIAN_POINT ( 'NONE',  ( -194.9999999999999716, 9.999999999999976907, 3.000000000000000000 ) ) ;
#3831 = VECTOR ( 'NONE', #2174, 1000.000000000000000 ) ;
#3832 = CARTESIAN_POINT ( 'NONE',  ( 1.846822687350017311, 10.23524390843949483, -7.075150813727003829 ) ) ;
#3833 = LINE ( 'NONE', #9659, #1671 ) ;
#3834 = EDGE_CURVE ( 'NONE', #4049, #9141, #14000, .T. ) ;
#3835 = CARTESIAN_POINT ( 'NONE',  ( 2.636624412715137922, -14.46769361191291559, 6.973567714907789927 ) ) ;
#3836 = CARTESIAN_POINT ( 'NONE',  ( 3.950837973638677170, 10.51028938476232355, -10.05648675950114956 ) ) ;
#3838 = ORIENTED_EDGE ( 'NONE', *, *, #17337, .T. ) ;
#3837 = CARTESIAN_POINT ( 'NONE',  ( 2.320521194581854463, 13.71278319227944920, 7.743190876766304243 ) ) ;
#3839 = LINE ( 'NONE', #11388, #10292 ) ;
#3840 = EDGE_CURVE ( 'NONE', #6348, #78, #3549, .T. ) ;
#3841 = AXIS2_PLACEMENT_3D ( 'NONE', #17972, #12233, #16622 ) ;
#3842 = CARTESIAN_POINT ( 'NONE',  ( 0.3148208552358962020, -11.24855514421869529, -7.888357771040825028 ) ) ;
#3843 = CARTESIAN_POINT ( 'NONE',  ( 0.3145734862173232838, -3.953068532979906458, -13.15783074029282673 ) ) ;
#3844 = STYLED_ITEM ( 'NONE', ( #14296 ), #10845 ) ;
#3845 = ORIENTED_EDGE ( 'NONE', *, *, #18010, .T. ) ;
#3846 = EDGE_LOOP ( 'NONE', ( #5583, #16320, #4399, #5039 ) ) ;
#3847 = CARTESIAN_POINT ( 'NONE',  ( 0.000000000000000000, 0.000000000000000000, 10.50000000000000000 ) ) ;
#3848 = ORIENTED_EDGE ( 'NONE', *, *, #6525, .F. ) ;
#3849 = CARTESIAN_POINT ( 'NONE',  ( 0.3142011359265305948, -8.382042760265827397, -10.88514493056451471 ) ) ;
#3850 = CARTESIAN_POINT ( 'NONE',  ( 1.959283090834842200, 10.53516775895160507, 6.829027319138286423 ) ) ;
#3851 =( NAMED_UNIT ( * ) SI_UNIT ( $, .STERADIAN. ) SOLID_ANGLE_UNIT ( ) );
#3852 = FACE_OUTER_BOUND ( 'NONE', #6088, .T. ) ;
#3853 = CARTESIAN_POINT ( 'NONE',  ( -1.500000000000001332, 6.799999999999999822, 5.000000000000000000 ) ) ;
#3854 = CIRCLE ( 'NONE', #6899, 5.000000000000000888 ) ;
#3855 = CARTESIAN_POINT ( 'NONE',  ( 2.353870697619109720, 0.7635393531608140050, -12.92712089195301850 ) ) ;
#3856 = APPLICATION_PROTOCOL_DEFINITION ( 'draft international standard', 'automotive_design', 1998, #14375 ) ;
#3857 = STYLED_ITEM ( 'NONE', ( #12344 ), #14891 ) ;
#3858 =( NAMED_UNIT ( * ) PLANE_ANGLE_UNIT ( ) SI_UNIT ( $, .RADIAN. ) );
#3859 = DIRECTION ( 'NONE',  ( 0.000000000000000000, 0.000000000000000000, 1.000000000000000000 ) ) ;
#3860 = DIRECTION ( 'NONE',  ( 0.000000000000000000, -0.000000000000000000, 1.000000000000000000 ) ) ;
#3861 =( BOUNDED_SURFACE ( )  B_SPLINE_SURFACE ( 3, 1, ( 
 ( #2172, #10688 ),
 ( #4946, #8009 ),
 ( #2255, #12389 ),
 ( #12215, #10778 ) ),
 .UNSPECIFIED., .F., .F., .T. ) 
 B_SPLINE_SURFACE_WITH_KNOTS ( ( 4, 4 ),
 ( 2, 2 ),
 ( 0.000000000000000000, 1.000000000000000000 ),
 ( 0.000000000000000000, 1.000000000000000000 ),
 .UNSPECIFIED. ) 
 GEOMETRIC_REPRESENTATION_ITEM ( )  RATIONAL_B_SPLINE_SURFACE ( (
 ( 1.000000000000000000, 1.000000000000000000),
 ( 0.7792777138730160313, 0.9689936506012927220),
 ( 0.7792777138730160313, 0.9689936506012927220),
 ( 1.000000000000000000, 1.000000000000000000) ) ) 
 REPRESENTATION_ITEM ( '' )  SURFACE ( )  );
#3862 =( BOUNDED_SURFACE ( )  B_SPLINE_SURFACE ( 3, 1, ( 
 ( #14333, #2938 ),
 ( #8688, #11471 ),
 ( #18716, #18816 ),
 ( #14516, #5919 ) ),
 .UNSPECIFIED., .F., .F., .T. ) 
 B_SPLINE_SURFACE_WITH_KNOTS ( ( 4, 4 ),
 ( 2, 2 ),
 ( 0.000000000000000000, 1.000000000000000000 ),
 ( 0.000000000000000000, 1.000000000000000000 ),
 .UNSPECIFIED. ) 
 GEOMETRIC_REPRESENTATION_ITEM ( )  RATIONAL_B_SPLINE_SURFACE ( (
 ( 1.000000000000000000, 1.000000000000000000),
 ( 0.9593108457356467333, 0.9995965569486454649),
 ( 0.9593108457356467333, 0.9995965569486454649),
 ( 1.000000000000000000, 1.000000000000000000) ) ) 
 REPRESENTATION_ITEM ( '' )  SURFACE ( )  );
#3863 = CARTESIAN_POINT ( 'NONE',  ( 0.3939875929385635578, -4.930599594904470528, -12.90850834464105645 ) ) ;
#3864 = CARTESIAN_POINT ( 'NONE',  ( 0.3095370825347224519, 4.681152801286160070, 12.91933430393609861 ) ) ;
#3865 = EDGE_CURVE ( 'NONE', #10362, #17016, #8830, .T. ) ;
#3866 = EDGE_CURVE ( 'NONE', #11500, #1343, #12189, .T. ) ;
#3867 = EDGE_CURVE ( 'NONE', #7021, #1472, #15580, .T. ) ;
#3868 = VECTOR ( 'NONE', #7669, 1000.000000000000114 ) ;
#3869 = CARTESIAN_POINT ( 'NONE',  ( 0.4862570985993235340, -11.67702470553359539, -7.559321496869553236 ) ) ;
#3870 = CARTESIAN_POINT ( 'NONE',  ( 2.123976203522053297, -6.261444813538658671, 14.31368049382967556 ) ) ;
#3871 = ORIENTED_EDGE ( 'NONE', *, *, #5215, .T. ) ;
#3872 = ORIENTED_EDGE ( 'NONE', *, *, #13334, .F. ) ;
#3873 = VERTEX_POINT ( 'NONE', #3150 ) ;
#3874 = ORIENTED_EDGE ( 'NONE', *, *, #13221, .T. ) ;
#3875 = CIRCLE ( 'NONE', #9061, 5.000000000000000000 ) ;
#3876 = CARTESIAN_POINT ( 'NONE',  ( 0.3142011359265333148, 11.33549115679423736, 7.762194356530812023 ) ) ;
#3877 = VECTOR ( 'NONE', #16207, 999.9999999999998863 ) ;
#3878 = DIRECTION ( 'NONE',  ( 0.000000000000000000, 0.000000000000000000, -1.000000000000000000 ) ) ;
#3879 = CARTESIAN_POINT ( 'NONE',  ( 0.000000000000000000, -2.500000000000000444, -16.99999999999999645 ) ) ;
#3880 = AXIS2_PLACEMENT_3D ( 'NONE', #1268, #18571, #5476 ) ;
#3881 = AXIS2_PLACEMENT_3D ( 'NONE', #8923, #13711, #7705 ) ;
#3882 = DIRECTION ( 'NONE',  ( 0.000000000000000000, 0.000000000000000000, 1.000000000000000000 ) ) ;
#3883 = CARTESIAN_POINT ( 'NONE',  ( 0.3095370825347224519, 13.73357284481724783, 0.4597470195090653799 ) ) ;
#3884 = CARTESIAN_POINT ( 'NONE',  ( 0.3142011359265295956, -0.3830873813805367734, -13.73310835363015059 ) ) ;
#3885 = CARTESIAN_POINT ( 'NONE',  ( 16.56872352241294521, 0.001821578298044641397, 0.01027347319884442528 ) ) ;
#3886 = EDGE_CURVE ( 'NONE', #11883, #473, #13077, .T. ) ;
#3887 = CARTESIAN_POINT ( 'NONE',  ( 0.4754618798421162973, 12.98792082933644743, 5.007009103465295929 ) ) ;
#3888 = EDGE_CURVE ( 'NONE', #8289, #18437, #16467, .T. ) ;
#3889 = ORIENTED_EDGE ( 'NONE', *, *, #5137, .F. ) ;
#3890 = EDGE_CURVE ( 'NONE', #13188, #11529, #88, .T. ) ;
#3891 = EDGE_CURVE ( 'NONE', #10554, #17590, #3923, .T. ) ;
#3892 = EDGE_LOOP ( 'NONE', ( #7918, #9491, #3226, #5493 ) ) ;
#3893 = VERTEX_POINT ( 'NONE', #5074 ) ;
#3894 = ORIENTED_EDGE ( 'NONE', *, *, #4468, .F. ) ;
#3895 = CARTESIAN_POINT ( 'NONE',  ( 1.846138399168762101, 3.446241763653166590, -11.95493567637846866 ) ) ;
#3896 = CARTESIAN_POINT ( 'NONE',  ( 1.560000000000000053, 1.732050807568878747, 7.017607234860990640E-28 ) ) ;
#3897 = CARTESIAN_POINT ( 'NONE',  ( 1.342453679581834924, -12.51077660954471504, 7.902645620902405632 ) ) ;
#3898 = CARTESIAN_POINT ( 'NONE',  ( 5.000000000000004441, -27.00000000000000000, 31.00000000000000000 ) ) ;
#3899 = CARTESIAN_POINT ( 'NONE',  ( 1.847034903785828019, -7.498375632854680006, 9.929438108952115982 ) ) ;
#3900 = EDGE_LOOP ( 'NONE', ( #5999, #4562 ) ) ;
#3901 = DIRECTION ( 'NONE',  ( -0.7561779333270775005, 0.1688126975276644792, -0.6322161072786924851 ) ) ;
#3902 = CARTESIAN_POINT ( 'NONE',  ( 1.846138399168762101, 0.4167076046095548603, 12.43476674860266762 ) ) ;
#3903 = CARTESIAN_POINT ( 'NONE',  ( 1.070106460717605401, 7.499999999999933387, -13.06798451319513532 ) ) ;
#3904 = LINE ( 'NONE', #6866, #16080 ) ;
#3905 = B_SPLINE_CURVE_WITH_KNOTS ( 'NONE', 3,
 ( #14282, #14365, #18661, #1083, #10066, #2694 ),
 .UNSPECIFIED., .F., .F.,
 ( 4, 2, 4 ),
 ( 3.499941646806256644E-17, 0.0001825746017570581273, 0.0003651492035140812891 ),
 .UNSPECIFIED. ) ;
#3906 = CIRCLE ( 'NONE', #17034, 5.000000000000000000 ) ;
#3907 = LINE ( 'NONE', #6690, #12971 ) ;
#3908 = CARTESIAN_POINT ( 'NONE',  ( 1.847461586945732925, 3.877048136045379234, 11.82388984758120287 ) ) ;
#3909 = CARTESIAN_POINT ( 'NONE',  ( 16.56753206892534891, 0.009389754735542245323, 0.001421777558675984534 ) ) ;
#3910 = CARTESIAN_POINT ( 'NONE',  ( 2.636624412716062515, -6.973567714909003179, -14.46769361191335790 ) ) ;
#3911 = ORIENTED_EDGE ( 'NONE', *, *, #14218, .F. ) ;
#3913 = ORIENTED_EDGE ( 'NONE', *, *, #17570, .T. ) ;
#3912 = FACE_OUTER_BOUND ( 'NONE', #7626, .T. ) ;
#3914 = CARTESIAN_POINT ( 'NONE',  ( 3.074695600507254767, -11.23985886659442635, 10.75417554975694578 ) ) ;
#3915 = ADVANCED_FACE ( 'NONE', ( #18266 ), #2298, .F. ) ;
#3916 = CARTESIAN_POINT ( 'NONE',  ( 0.4862570985993235340, 13.89016912371017476, 0.7479633556562934604 ) ) ;
#3917 = ORIENTED_EDGE ( 'NONE', *, *, #14530, .F. ) ;
#3918 = DIRECTION ( 'NONE',  ( -0.000000000000000000, -0.000000000000000000, 1.000000000000000000 ) ) ;
#3919 = CARTESIAN_POINT ( 'NONE',  ( 1.847461586945731371, -12.44326124954594448, 0.03350899125588503030 ) ) ;
#3920 = DIRECTION ( 'NONE',  ( -1.000000000000000000, -0.000000000000000000, -0.000000000000000000 ) ) ;
#3921 = ORIENTED_EDGE ( 'NONE', *, *, #18762, .T. ) ;
#3922 = CARTESIAN_POINT ( 'NONE',  ( 2.320520222537280297, -10.64885284335050741, 11.60169517779339898 ) ) ;
#3923 = LINE ( 'NONE', #18174, #6099 ) ;
#3924 = DIRECTION ( 'NONE',  ( 0.000000000000000000, 0.000000000000000000, -1.000000000000000000 ) ) ;
#3925 = LINE ( 'NONE', #9749, #13599 ) ;
#3926 = DIRECTION ( 'NONE',  ( -0.4246593920385851040, -0.1376957914266804250, 0.8948208031649687033 ) ) ;
#3927 = EDGE_CURVE ( 'NONE', #10438, #18549, #1509, .T. ) ;
#3928 = CARTESIAN_POINT ( 'NONE',  ( -105.8941953964643261, -81.60345299795268659, -89.13679372318456728 ) ) ;
#3929 = ORIENTED_EDGE ( 'NONE', *, *, #15678, .F. ) ;
#3930 = EDGE_CURVE ( 'NONE', #4935, #7817, #11816, .T. ) ;
#3931 = AXIS2_PLACEMENT_3D ( 'NONE', #4340, #14651, #14743 ) ;
#3932 = CARTESIAN_POINT ( 'NONE',  ( 16.58200780006414732, -0.007066318000005944282, 0.008650561019685880718 ) ) ;
#3934 = ORIENTED_EDGE ( 'NONE', *, *, #9260, .F. ) ;
#3933 = CARTESIAN_POINT ( 'NONE',  ( 16.56872352241294521, -0.009382111268607402216, -0.004564908236399935551 ) ) ;
#3935 = CARTESIAN_POINT ( 'NONE',  ( -199.9999999999999716, -10.00000000000002665, 6.000000000000000000 ) ) ;
#3936 = B_SPLINE_CURVE_WITH_KNOTS ( 'NONE', 3,
 ( #10502, #13552, #475, #16339, #9254, #17967, #3518, #3220, #6302, #3421, #4866, #12135, #15083 ),
 .UNSPECIFIED., .F., .F.,
 ( 4, 3, 3, 3, 4 ),
 ( 0.000000000000000000, 0.0002299804304191505879, 0.0004599608082120279365, 0.0006467586077648024507, 0.0008336169836825989407 ),
 .UNSPECIFIED. ) ;
#3937 = CARTESIAN_POINT ( 'NONE',  ( 0.3170788640506441158, -13.02120094575831288, 4.392045232375760833 ) ) ;
#3938 = CARTESIAN_POINT ( 'NONE',  ( 2.320520222536567090, 11.60169517779319293, 10.64885284334832960 ) ) ;
#3939 =( BOUNDED_SURFACE ( )  B_SPLINE_SURFACE ( 3, 1, ( 
 ( #5969, #7617 ),
 ( #17343, #11805 ),
 ( #6074, #17641 ),
 ( #1488, #17537 ) ),
 .UNSPECIFIED., .F., .F., .T. ) 
 B_SPLINE_SURFACE_WITH_KNOTS ( ( 4, 4 ),
 ( 2, 2 ),
 ( 0.000000000000000000, 1.000000000000000000 ),
 ( 0.000000000000000000, 1.000000000000000000 ),
 .UNSPECIFIED. ) 
 GEOMETRIC_REPRESENTATION_ITEM ( )  RATIONAL_B_SPLINE_SURFACE ( (
 ( 1.000000000000000000, 1.000000000000000000),
 ( 0.7792777138730160313, 0.9689936506012927220),
 ( 0.7792777138730160313, 0.9689936506012927220),
 ( 1.000000000000000000, 1.000000000000000000) ) ) 
 REPRESENTATION_ITEM ( '' )  SURFACE ( )  );
#3940 = ORIENTED_EDGE ( 'NONE', *, *, #13397, .F. ) ;
#3941 = CARTESIAN_POINT ( 'NONE',  ( 6.538348415311010520, 2.499999999999998668, -12.00000000000000000 ) ) ;
#3942 = DIRECTION ( 'NONE',  ( 0.000000000000000000, 1.000000000000000000, 0.000000000000000000 ) ) ;
#3943 = ORIENTED_EDGE ( 'NONE', *, *, #491, .T. ) ;
#3944 = DIRECTION ( 'NONE',  ( 0.000000000000000000, 0.000000000000000000, -1.000000000000000000 ) ) ;
#3945 = CARTESIAN_POINT ( 'NONE',  ( 18.30499999999999972, 3.061616997868382648E-16, -2.499999999999999556 ) ) ;
#3946 = DIRECTION ( 'NONE',  ( 1.000000000000000000, 0.000000000000000000, 0.000000000000000000 ) ) ;
#3947 = AXIS2_PLACEMENT_3D ( 'NONE', #7345, #5886, #11920 ) ;
#3948 = CARTESIAN_POINT ( 'NONE',  ( 0.3150686449036064207, -11.02450593298024195, 8.199336701264503091 ) ) ;
#3950 = CARTESIAN_POINT ( 'NONE',  ( 16.56872352241294521, 0.007240717549633990044, -0.007512283835805476720 ) ) ;
#3949 = AXIS2_PLACEMENT_3D ( 'NONE', #5355, #15392, #10924 ) ;
#3951 = ADVANCED_FACE ( 'NONE', ( #4012 ), #11104, .T. ) ;
#3952 = APPLICATION_PROTOCOL_DEFINITION ( 'draft international standard', 'automotive_design', 1998, #3119 ) ;
#3953 = AXIS2_PLACEMENT_3D ( 'NONE', #5234, #15192, #932 ) ;
#3954 = CARTESIAN_POINT ( 'NONE',  ( -199.9999999999999716, -5.000000000000024869, 3.000000000000000000 ) ) ;
#3955 = EDGE_CURVE ( 'NONE', #5950, #2340, #4058, .T. ) ;
#3956 = CARTESIAN_POINT ( 'NONE',  ( 0.3720661004400037664, -12.89739157014188997, -4.951033743989776248 ) ) ;
#3957 = CARTESIAN_POINT ( 'NONE',  ( 1.846138399168762101, -7.646096044339819819, -9.815003036200495856 ) ) ;
#3958 = DIRECTION ( 'NONE',  ( 1.000000000000000000, 0.000000000000000000, 0.000000000000000000 ) ) ;
#3959 = DIRECTION ( 'NONE',  ( -0.000000000000000000, -1.000000000000000000, -0.000000000000000000 ) ) ;
#3960 = LINE ( 'NONE', #16776, #13659 ) ;
#3961 = VERTEX_POINT ( 'NONE', #5168 ) ;
#3962 = VERTEX_POINT ( 'NONE', #3828 ) ;
#3963 = VERTEX_POINT ( 'NONE', #8326 ) ;
#3964 = EDGE_LOOP ( 'NONE', ( #928, #17965, #17196, #1901 ) ) ;
#3965 = DIRECTION ( 'NONE',  ( 0.000000000000000000, -0.000000000000000000, 1.000000000000000000 ) ) ;
#3966 = CYLINDRICAL_SURFACE ( 'NONE', #7563, 4.999999999999997335 ) ;
#3967 = EDGE_CURVE ( 'NONE', #421, #885, #12722, .T. ) ;
#3968 = CARTESIAN_POINT ( 'NONE',  ( 0.4754618798421162973, 5.007009103465432709, -12.98792082933639058 ) ) ;
#3969 = CARTESIAN_POINT ( 'NONE',  ( 2.002547531651519996, -11.75462648437098601, -4.532360870844453160 ) ) ;
#3970 =( BOUNDED_SURFACE ( )  B_SPLINE_SURFACE ( 3, 1, ( 
 ( #17129, #7099 ),
 ( #7199, #12917 ),
 ( #11499, #13011 ),
 ( #3950, #17316 ) ),
 .UNSPECIFIED., .F., .F., .T. ) 
 B_SPLINE_SURFACE_WITH_KNOTS ( ( 4, 4 ),
 ( 2, 2 ),
 ( 0.000000000000000000, 1.000000000000000000 ),
 ( 0.000000000000000000, 1.000000000000000000 ),
 .UNSPECIFIED. ) 
 GEOMETRIC_REPRESENTATION_ITEM ( )  RATIONAL_B_SPLINE_SURFACE ( (
 ( 1.000000000000000000, 1.000000000000000000),
 ( 0.9933953342250436691, 0.8357391271907733676),
 ( 0.9933953342250436691, 0.8357391271907733676),
 ( 1.000000000000000000, 1.000000000000000000) ) ) 
 REPRESENTATION_ITEM ( '' )  SURFACE ( )  );
#3971 =( NAMED_UNIT ( * ) PLANE_ANGLE_UNIT ( ) SI_UNIT ( $, .RADIAN. ) );
#3972 = CARTESIAN_POINT ( 'NONE',  ( 0.4862570985993235340, -12.97920246947883172, 5.003653737315437944 ) ) ;
#3973 = CARTESIAN_POINT ( 'NONE',  ( 2.747332970342022840, -7.289199830147212289, 14.63517873738944708 ) ) ;
#3974 = CARTESIAN_POINT ( 'NONE',  ( 0.3137051932979775248, -12.91601973349273891, 4.679953077377436266 ) ) ;
#3975 = FACE_OUTER_BOUND ( 'NONE', #6217, .T. ) ;
#3976 = ORIENTED_EDGE ( 'NONE', *, *, #3159, .T. ) ;
#3977 = B_SPLINE_CURVE_WITH_KNOTS ( 'NONE', 3,
 ( #16893, #7317, #6961, #16192, #6066, #14656, #12771, #7507, #8922, #15631, #1110, #3175, #10459 ),
 .UNSPECIFIED., .F., .F.,
 ( 4, 3, 3, 3, 4 ),
 ( 3.127317220692750759E-18, 0.0002299804304191474438, 0.0004599608082120254971, 0.0006467586077648028843, 0.0008336169836825993744 ),
 .UNSPECIFIED. ) ;
#3978 = B_SPLINE_CURVE_WITH_KNOTS ( 'NONE', 3,
 ( #10286, #17751, #449, #12111, #17845, #13532 ),
 .UNSPECIFIED., .F., .F.,
 ( 4, 2, 4 ),
 ( 0.000000000000000000, 0.001500839035891548753, 0.003001678071783097507 ),
 .UNSPECIFIED. ) ;
#3979 = VERTEX_POINT ( 'NONE', #8145 ) ;
#3980 = ORIENTED_EDGE ( 'NONE', *, *, #8436, .F. ) ;
#3981 = EDGE_LOOP ( 'NONE', ( #17144, #1208, #10696, #2884 ) ) ;
#3982 = DIRECTION ( 'NONE',  ( 0.7071067818211348444, 8.659560554583479511E-17, 0.7071067805519601901 ) ) ;
#3983 = CARTESIAN_POINT ( 'NONE',  ( 3.353306896162455697, -12.78841260990234119, -5.573563251762232440 ) ) ;
#3984 = CARTESIAN_POINT ( 'NONE',  ( 6.538348415311014072, -7.500000000000000888, -16.99999999999999645 ) ) ;
#3985 = CARTESIAN_POINT ( 'NONE',  ( 8.522092701127531811, -6.722964936702111594, 1.786985377232005900 ) ) ;
#3986 = ORIENTED_EDGE ( 'NONE', *, *, #15577, .T. ) ;
#3987 = DIRECTION ( 'NONE',  ( -1.000000000000000000, 0.000000000000000000, 0.000000000000000000 ) ) ;
#3988 = EDGE_CURVE ( 'NONE', #9141, #10419, #6577, .T. ) ;
#3989 = EDGE_CURVE ( 'NONE', #369, #14405, #2473, .T. ) ;
#3990 = CARTESIAN_POINT ( 'NONE',  ( 1.846524061778021419, -11.71897913237546263, -4.180439405448447054 ) ) ;
#3991 = EDGE_CURVE ( 'NONE', #14770, #13012, #606, .T. ) ;
#3992 = CARTESIAN_POINT ( 'NONE',  ( 5.029793280284322599, 7.499999999999999112, -16.81208494724229396 ) ) ;
#3993 = LINE ( 'NONE', #18333, #15180 ) ;
#3994 = CARTESIAN_POINT ( 'NONE',  ( 2.123976203522053741, -15.54801196254788209, 1.531817366691698545 ) ) ;
#3995 = FACE_OUTER_BOUND ( 'NONE', #9987, .T. ) ;
#3996 = CARTESIAN_POINT ( 'NONE',  ( 0.4754618798421162973, -7.564402563418551217, 11.68486377711963975 ) ) ;
#3997 = CARTESIAN_POINT ( 'NONE',  ( 3.353306896162456585, 5.573563251762281290, -12.78841260990232165 ) ) ;
#3998 = ORIENTED_EDGE ( 'NONE', *, *, #15156, .T. ) ;
#4000 = VERTEX_POINT ( 'NONE', #2388 ) ;
#3999 = CARTESIAN_POINT ( 'NONE',  ( 2.747332970342022840, -11.45495994260709161, -11.66639548242820190 ) ) ;
#4001 = CARTESIAN_POINT ( 'NONE',  ( 16.56872352241294521, -0.004564908236400289435, -0.009382111268606239951 ) ) ;
#4002 = B_SPLINE_CURVE_WITH_KNOTS ( 'NONE', 3,
 ( #15134, #7978, #12622, #4911, #5088, #3465 ),
 .UNSPECIFIED., .F., .F.,
 ( 4, 2, 4 ),
 ( 0.000000000000000000, 0.001656992708822831520, 0.003313985417645663040 ),
 .UNSPECIFIED. ) ;
#4003 = CONICAL_SURFACE ( 'NONE', #13459, 14.54644660717763927, 0.8559913436420816257 ) ;
#4004 = CARTESIAN_POINT ( 'NONE',  ( 3.950837973638668288, 14.41405733518061538, -1.958075594453841273 ) ) ;
#4005 = ORIENTED_EDGE ( 'NONE', *, *, #3550, .T. ) ;
#4006 = CARTESIAN_POINT ( 'NONE',  ( 3.950837973638668288, 0.000000000000000000, 0.000000000000000000 ) ) ;
#4007 = CARTESIAN_POINT ( 'NONE',  ( -6.144877202871137811, -7.499999999999999112, -12.52666336607935094 ) ) ;
#4008 = CARTESIAN_POINT ( 'NONE',  ( -199.9999999999999716, 4.999999999999974243, -2.000000000000000000 ) ) ;
#4009 = LINE ( 'NONE', #4106, #1700 ) ;
#4010 = ORIENTED_EDGE ( 'NONE', *, *, #1534, .F. ) ;
#4011 = CARTESIAN_POINT ( 'NONE',  ( 2.750000000000000000, 0.000000000000000000, 11.00000000000000000 ) ) ;
#4012 = FACE_OUTER_BOUND ( 'NONE', #17823, .T. ) ;
#4013 = B_SPLINE_CURVE_WITH_KNOTS ( 'NONE', 3,
 ( #2540, #15555, #12324, #5242, #2370, #6780 ),
 .UNSPECIFIED., .F., .F.,
 ( 4, 2, 4 ),
 ( 0.000000000000000000, 0.0001828790815886951050, 0.0003657581631773902100 ),
 .UNSPECIFIED. ) ;
#4014 = FACE_OUTER_BOUND ( 'NONE', #15355, .T. ) ;
#4015 = CARTESIAN_POINT ( 'NONE',  ( 1.846138399168762101, 10.30487220521580305, -6.971848976710897539 ) ) ;
#4016 = CARTESIAN_POINT ( 'NONE',  ( 0.000000000000000000, 0.000000000000000000, 7.000000000000000000 ) ) ;
#4017 = EDGE_CURVE ( 'NONE', #6216, #17983, #18585, .T. ) ;
#4018 = EDGE_CURVE ( 'NONE', #14993, #13051, #8237, .T. ) ;
#4019 = CARTESIAN_POINT ( 'NONE',  ( 16.57778382496167424, 0.002851818597093403688, 0.01466529584256672306 ) ) ;
#4020 = AXIS2_PLACEMENT_3D ( 'NONE', #7263, #15188, #7652 ) ;
#4021 = DIRECTION ( 'NONE',  ( -1.000000000000000000, 0.000000000000000000, -0.000000000000000000 ) ) ;
#4023 = ORIENTED_EDGE ( 'NONE', *, *, #18359, .T. ) ;
#4022 = CARTESIAN_POINT ( 'NONE',  ( -199.9999999999999716, -5.000000000000024869, 6.000000000000000000 ) ) ;
#4024 = CARTESIAN_POINT ( 'NONE',  ( 2.353870697619111496, -4.720869121224215093, 12.05847592522641953 ) ) ;
#4025 = EDGE_CURVE ( 'NONE', #15040, #10542, #4875, .T. ) ;
#4026 = CARTESIAN_POINT ( 'NONE',  ( 0.3137051932979792457, -12.91601973349266963, -4.679953077377624560 ) ) ;
#4027 = VERTEX_POINT ( 'NONE', #17582 ) ;
#4028 = CARTESIAN_POINT ( 'NONE',  ( -199.9999999999999716, 4.999999999999974243, 11.00000000000000000 ) ) ;
#4029 = CARTESIAN_POINT ( 'NONE',  ( 2.636624412716062515, -6.973567714909003179, -14.46769361191335790 ) ) ;
#4030 = ORIENTED_EDGE ( 'NONE', *, *, #3967, .F. ) ;
#4031 = DIRECTION ( 'NONE',  ( -0.000000000000000000, 0.5000000000000003331, -0.8660254037844384856 ) ) ;
#4032 = LINE ( 'NONE', #2490, #2714 ) ;
#4033 = CARTESIAN_POINT ( 'NONE',  ( 0.3137051932979809665, -3.805684345189881856, 13.20008686438104739 ) ) ;
#4034 = AXIS2_PLACEMENT_3D ( 'NONE', #11606, #13831, #5659 ) ;
#4035 = EDGE_CURVE ( 'NONE', #473, #1860, #8689, .T. ) ;
#4036 = CARTESIAN_POINT ( 'NONE',  ( 0.3137051932979775248, -0.4596302728638797519, -13.73004976592202553 ) ) ;
#4037 = DIRECTION ( 'NONE',  ( -1.000000000000000000, 0.000000000000000000, -0.000000000000000000 ) ) ;
#4038 = UNCERTAINTY_MEASURE_WITH_UNIT (LENGTH_MEASURE( 1.000000000000000082E-05 ), #2961, 'distance_accuracy_value', 'NONE');
#4039 = ORIENTED_EDGE ( 'NONE', *, *, #17573, .F. ) ;
#4040 = EDGE_CURVE ( 'NONE', #15271, #15610, #12892, .T. ) ;
#4041 = EDGE_CURVE ( 'NONE', #3145, #3962, #14334, .T. ) ;
#4042 =( NAMED_UNIT ( * ) PLANE_ANGLE_UNIT ( ) SI_UNIT ( $, .RADIAN. ) );
#4043 = CARTESIAN_POINT ( 'NONE',  ( -1.500000000000000888, 4.769696007084728073, -3.000000000000000000 ) ) ;
#4044 = CARTESIAN_POINT ( 'NONE',  ( 0.3148208552358916501, -12.99355031785208681, 4.463611911212169936 ) ) ;
#4045 =( BOUNDED_SURFACE ( )  B_SPLINE_SURFACE ( 3, 1, ( 
 ( #8781, #8586 ),
 ( #7359, #1606 ),
 ( #10402, #13263 ),
 ( #13169, #17572 ) ),
 .UNSPECIFIED., .F., .F., .T. ) 
 B_SPLINE_SURFACE_WITH_KNOTS ( ( 4, 4 ),
 ( 2, 2 ),
 ( 0.000000000000000000, 1.000000000000000000 ),
 ( 0.000000000000000000, 1.000000000000000000 ),
 .UNSPECIFIED. ) 
 GEOMETRIC_REPRESENTATION_ITEM ( )  RATIONAL_B_SPLINE_SURFACE ( (
 ( 1.000000000000000000, 1.000000000000000000),
 ( 0.9933953342250438912, 0.8357391271907739227),
 ( 0.9933953342250438912, 0.8357391271907739227),
 ( 1.000000000000000000, 1.000000000000000000) ) ) 
 REPRESENTATION_ITEM ( '' )  SURFACE ( )  );
#4046 = CARTESIAN_POINT ( 'NONE',  ( 1.846138399168762101, 0.4167076046095548603, 12.43476674860266762 ) ) ;
#4047 = CARTESIAN_POINT ( 'NONE',  ( -194.9999999999999716, 9.999999999999973355, 6.000000000000000000 ) ) ;
#4048 = CYLINDRICAL_SURFACE ( 'NONE', #7572, 2.749999999999997335 ) ;
#4049 = VERTEX_POINT ( 'NONE', #15950 ) ;
#4050 = CARTESIAN_POINT ( 'NONE',  ( 0.3150686449036038117, 11.02450593298030412, -8.199336701264417826 ) ) ;
#4051 = FACE_OUTER_BOUND ( 'NONE', #17350, .T. ) ;
#4052 = EDGE_LOOP ( 'NONE', ( #18755, #15723, #15542, #5809 ) ) ;
#4053 = EDGE_CURVE ( 'NONE', #8937, #15252, #14748, .T. ) ;
#4054 = EDGE_LOOP ( 'NONE', ( #15434, #6932, #5823, #12054 ) ) ;
#4055 = EDGE_LOOP ( 'NONE', ( #11331, #17472, #4124, #8309 ) ) ;
#4056 = CARTESIAN_POINT ( 'NONE',  ( 3.512766787570746452, -10.40533104696126898, -10.87507422923902034 ) ) ;
#4057 = ORIENTED_EDGE ( 'NONE', *, *, #373, .T. ) ;
#4058 = B_SPLINE_CURVE_WITH_KNOTS ( 'NONE', 3,
 ( #18540, #16743, #3642, #11291, #16829, #12436 ),
 .UNSPECIFIED., .F., .F.,
 ( 4, 2, 4 ),
 ( 1.084202172485504314E-19, 0.001657017934711308349, 0.003314035869422615830 ),
 .UNSPECIFIED. ) ;
#4059 = CIRCLE ( 'NONE', #11680, 4.000000000000000000 ) ;
#4060 = DIRECTION ( 'NONE',  ( 0.000000000000000000, 0.000000000000000000, 1.000000000000000000 ) ) ;
#4061 = CARTESIAN_POINT ( 'NONE',  ( 0.3142014840576502488, 13.17932813834300099, -3.879477880151306568 ) ) ;
#4062 = CARTESIAN_POINT ( 'NONE',  ( -205.0000000000000000, 4.999999999999974243, 3.000000000000002665 ) ) ;
#4063 = CARTESIAN_POINT ( 'NONE',  ( 2.636624412716062515, -6.973567714909003179, -14.46769361191335790 ) ) ;
#4064 =( NAMED_UNIT ( * ) SI_UNIT ( $, .STERADIAN. ) SOLID_ANGLE_UNIT ( ) );
#4065 = CARTESIAN_POINT ( 'NONE',  ( 0.3137051932979757485, 7.698472063774634222, -11.37800749014122736 ) ) ;
#4066 = CARTESIAN_POINT ( 'NONE',  ( 1.342453679581834924, 3.649820028552932971, -14.34050741580202981 ) ) ;
#4067 = CARTESIAN_POINT ( 'NONE',  ( 0.4754618798421171855, -8.775436892861030458, -10.80499583390522744 ) ) ;
#4068 = CARTESIAN_POINT ( 'NONE',  ( 1.846138399168762101, -12.43476674860266940, 0.4167076046095114505 ) ) ;
#4069 = CIRCLE ( 'NONE', #727, 0.5000000000000000000 ) ;
#4070 = EDGE_CURVE ( 'NONE', #8886, #12927, #18639, .T. ) ;
#4071 = AXIS2_PLACEMENT_3D ( 'NONE', #11262, #17259, #12677 ) ;
#4072 = ORIENTED_EDGE ( 'NONE', *, *, #8028, .T. ) ;
#4073 = EDGE_LOOP ( 'NONE', ( #15628, #15422, #18222, #4846 ) ) ;
#4074 = ADVANCED_FACE ( 'NONE', ( #17288 ), #5618, .F. ) ;
#4075 = ORIENTED_EDGE ( 'NONE', *, *, #14290, .F. ) ;
#4076 = ORIENTED_EDGE ( 'NONE', *, *, #1185, .F. ) ;
#4077 = CARTESIAN_POINT ( 'NONE',  ( 2.002547531651519996, -12.17374746633580784, 3.242439124566603326 ) ) ;
#4078 = CARTESIAN_POINT ( 'NONE',  ( 0.3939875929385642239, -0.7003304234512184312, -13.80036004410494854 ) ) ;
#4079 = CARTESIAN_POINT ( 'NONE',  ( 2.636624412716062960, -2.161493821598612808, -15.91454522070331912 ) ) ;
#4080 = VERTEX_POINT ( 'NONE', #5311 ) ;
#4081 = FACE_OUTER_BOUND ( 'NONE', #8018, .T. ) ;
#4082 = DIRECTION ( 'NONE',  ( 0.000000000000000000, 0.000000000000000000, 1.000000000000000000 ) ) ;
#4083 = VECTOR ( 'NONE', #8661, 1000.000000000000000 ) ;
#4084 = CARTESIAN_POINT ( 'NONE',  ( 8.438534575730034959, 0.2320579683290127926, 6.862570336891076650 ) ) ;
#4085 = CARTESIAN_POINT ( 'NONE',  ( 0.8740779401509238822, -13.83508928787439096, -3.609949156401517367 ) ) ;
#4086 = DIRECTION ( 'NONE',  ( -1.000000000000000000, 0.000000000000000000, 0.000000000000000000 ) ) ;
#4087 = DIRECTION ( 'NONE',  ( -1.000000000000000000, -0.000000000000000000, -0.000000000000000000 ) ) ;
#4088 = FACE_OUTER_BOUND ( 'NONE', #13282, .T. ) ;
#4089 = DIRECTION ( 'NONE',  ( 1.601283208593975514E-16, -1.000000000000000000, 0.000000000000000000 ) ) ;
#4090 = CARTESIAN_POINT ( 'NONE',  ( 1.847380140988739594, -3.740232970470839913, 11.86779270755357807 ) ) ;
#4091 = ORIENTED_EDGE ( 'NONE', *, *, #2407, .F. ) ;
#4093 = ORIENTED_EDGE ( 'NONE', *, *, #10331, .F. ) ;
#4092 = PLANE ( 'NONE',  #226 ) ;
#4094 = DIRECTION ( 'NONE',  ( -0.000000000000000000, -0.000000000000000000, -1.000000000000000000 ) ) ;
#4095 = EDGE_CURVE ( 'NONE', #4709, #14938, #10917, .T. ) ;
#4096 = EDGE_CURVE ( 'NONE', #8123, #10867, #15534, .T. ) ;
#4097 = EDGE_CURVE ( 'NONE', #16458, #13316, #16307, .T. ) ;
#4098 = CARTESIAN_POINT ( 'NONE',  ( 0.3095370825347224519, 4.681152801286340370, -12.91933430393602933 ) ) ;
#4099 = VECTOR ( 'NONE', #2971, 1000.000000000000000 ) ;
#4100 = B_SPLINE_CURVE_WITH_KNOTS ( 'NONE', 3,
 ( #10365, #4730, #3177, #1867 ),
 .UNSPECIFIED., .F., .F.,
 ( 4, 4 ),
 ( 0.000000000000000000, 0.002004993803842355579 ),
 .UNSPECIFIED. ) ;
#4101 = CARTESIAN_POINT ( 'NONE',  ( 16.56782317627811096, 0.009814734722106368062, -0.0003415813796015080314 ) ) ;
#4102 = VERTEX_POINT ( 'NONE', #11378 ) ;
#4103 = CARTESIAN_POINT ( 'NONE',  ( 3.512766787570723803, -13.25664064834472100, -7.127386085302978458 ) ) ;
#4104 = DIRECTION ( 'NONE',  ( -0.000000000000000000, 0.000000000000000000, -1.000000000000000000 ) ) ;
#4105 = CARTESIAN_POINT ( 'NONE',  ( 2.636624412715384391, -11.60464335004044223, -11.10302021258006278 ) ) ;
#4106 = CARTESIAN_POINT ( 'NONE',  ( 8.522092701127531811, -4.388629235579615262, 5.397361180353127175 ) ) ;
#4107 = EDGE_LOOP ( 'NONE', ( #5226, #8780, #10476 ) ) ;
#4108 = CARTESIAN_POINT ( 'NONE',  ( 3.950837973638675393, 6.888253895133292559, 12.81214529934977797 ) ) ;
#4109 = CARTESIAN_POINT ( 'NONE',  ( 1.918921323896325193, 3.258415356426521026, 12.08297777410666285 ) ) ;
#4110 = CARTESIAN_POINT ( 'NONE',  ( 0.3137051932979792457, -13.73004976592201842, -0.4596302728641207813 ) ) ;
#4111 = DIRECTION ( 'NONE',  ( 0.000000000000000000, 0.000000000000000000, 1.000000000000000000 ) ) ;
#4112 = EDGE_CURVE ( 'NONE', #17568, #15056, #8596, .T. ) ;
#4113 = AXIS2_PLACEMENT_3D ( 'NONE', #17385, #10217, #11564 ) ;
#4114 = CARTESIAN_POINT ( 'NONE',  ( -194.9999999999999716, 9.999999999999973355, 3.000000000000002665 ) ) ;
#4115 = APPLICATION_CONTEXT ( 'automotive_design' ) ;
#4116 = VECTOR ( 'NONE', #16051, 1000.000000000000227 ) ;
#4117 = VECTOR ( 'NONE', #9256, 1000.000000000000000 ) ;
#4118 = DIRECTION ( 'NONE',  ( 0.7561779333270775005, -0.4122479608995778255, 0.5081796452863200919 ) ) ;
#4119 = CARTESIAN_POINT ( 'NONE',  ( 0.000000000000000000, 0.000000000000000000, 0.000000000000000000 ) ) ;
#4121 = ORIENTED_EDGE ( 'NONE', *, *, #8585, .F. ) ;
#4120 = CARTESIAN_POINT ( 'NONE',  ( 3.950837973638676281, 14.31366178983253512, 2.591948120961855118 ) ) ;
#4122 = CARTESIAN_POINT ( 'NONE',  ( 0.3132642857406563452, -0.5276792104583234444, 13.72733058964894326 ) ) ;
#4123 = EDGE_CURVE ( 'NONE', #16044, #1784, #17198, .T. ) ;
#4124 = ORIENTED_EDGE ( 'NONE', *, *, #8624, .T. ) ;
#4125 = CARTESIAN_POINT ( 'NONE',  ( 3.950837973638675393, -13.10350451991845055, 6.316429227969417859 ) ) ;
#4126 = EDGE_CURVE ( 'NONE', #8651, #10554, #11341, .T. ) ;
#4127 = AXIS2_PLACEMENT_3D ( 'NONE', #5076, #12438, #10928 ) ;
#4128 = PLANE ( 'NONE',  #14182 ) ;
#4129 = ORIENTED_EDGE ( 'NONE', *, *, #18031, .F. ) ;
#4130 = CARTESIAN_POINT ( 'NONE',  ( 0.3095370825347224519, 12.91933430393608084, 4.681152801286204479 ) ) ;
#4131 = DIRECTION ( 'NONE',  ( 2.891205793294679312E-16, -1.000000000000000000, 0.000000000000000000 ) ) ;
#4132 = CARTESIAN_POINT ( 'NONE',  ( 0.3151928476913592458, -4.245457024760312947, 13.06684726503524807 ) ) ;
#4133 = CARTESIAN_POINT ( 'NONE',  ( 0.3145729642390356351, -0.3065092323350255277, -13.73540280162741389 ) ) ;
#4134 = DIRECTION ( 'NONE',  ( -0.000000000000000000, -0.000000000000000000, -1.000000000000000000 ) ) ;
#4135 = EDGE_CURVE ( 'NONE', #12673, #911, #18818, .T. ) ;
#4136 = ORIENTED_EDGE ( 'NONE', *, *, #2680, .T. ) ;
#4137 = B_SPLINE_CURVE_WITH_KNOTS ( 'NONE', 3,
 ( #11537, #5782, #7139, #16122, #3003, #5685 ),
 .UNSPECIFIED., .F., .F.,
 ( 4, 2, 4 ),
 ( 0.000000000000000000, 0.001657017934711440188, 0.003314035869422880375 ),
 .UNSPECIFIED. ) ;
#4138 = ITEM_DEFINED_TRANSFORMATION ( 'NONE', 'NONE', #8151,  #2030 ) ;
#4139 = B_SPLINE_CURVE_WITH_KNOTS ( 'NONE', 3,
 ( #8632, #15894, #14179, #8360, #17054, #9865 ),
 .UNSPECIFIED., .F., .F.,
 ( 4, 2, 4 ),
 ( 3.556447555475521540E-17, 0.0001825746017570583171, 0.0003651492035140810723 ),
 .UNSPECIFIED. ) ;
#4140 =( NAMED_UNIT ( * ) PLANE_ANGLE_UNIT ( ) SI_UNIT ( $, .RADIAN. ) );
#4141 = CARTESIAN_POINT ( 'NONE',  ( 0.3095370825347234511, 0.4597470195092124290, -13.73357284481724250 ) ) ;
#4142 = CARTESIAN_POINT ( 'NONE',  ( 0.3137051932979775248, -12.91601973349273891, 4.679953077377436266 ) ) ;
#4143 = B_SPLINE_CURVE_WITH_KNOTS ( 'NONE', 3,
 ( #7443, #14500, #73, #13064, #16228, #5792 ),
 .UNSPECIFIED., .F., .F.,
 ( 4, 2, 4 ),
 ( 8.940560153363745023E-19, 0.0001828790815881870750, 0.0003657581631763732284 ),
 .UNSPECIFIED. ) ;
#4144 = CARTESIAN_POINT ( 'NONE',  ( 0.3137051932979792457, -10.83767969834809008, 8.442169467526815296 ) ) ;
#4145 = CARTESIAN_POINT ( 'NONE',  ( 16.56679352167444819, -0.008311568981097361419, 0.004162264567719621902 ) ) ;
#4146 = FACE_OUTER_BOUND ( 'NONE', #6470, .T. ) ;
#4147 = ORIENTED_EDGE ( 'NONE', *, *, #2090, .F. ) ;
#4148 = DIRECTION ( 'NONE',  ( -1.000000000000000000, -0.000000000000000000, -0.000000000000000000 ) ) ;
#4149 = CARTESIAN_POINT ( 'NONE',  ( 0.3720661004400040439, 8.694226082900595287, 10.73619472937705233 ) ) ;
#4150 = VERTEX_POINT ( 'NONE', #14996 ) ;
#4151 = ORIENTED_EDGE ( 'NONE', *, *, #11967, .T. ) ;
#4152 = CARTESIAN_POINT ( 'NONE',  ( 16.56753206892534891, 0.001421777558675947238, -0.009389754735542250527 ) ) ;
#4153 = EDGE_CURVE ( 'NONE', #18897, #5848, #15074, .T. ) ;
#4154 = VERTEX_POINT ( 'NONE', #11946 ) ;
#4155 = LINE ( 'NONE', #15804, #17789 ) ;
#4156 = EDGE_LOOP ( 'NONE', ( #15184, #15990, #2659, #571 ) ) ;
#4157 = AXIS2_PLACEMENT_3D ( 'NONE', #1017, #8029, #8208 ) ;
#4158 = MECHANICAL_DESIGN_GEOMETRIC_PRESENTATION_REPRESENTATION (  '', ( #6598 ), #503 ) ;
#4159 = LINE ( 'NONE', #9978, #18499 ) ;
#4160 = CARTESIAN_POINT ( 'NONE',  ( 2.320520222538103638, 6.542539914241700671, -14.32454429810417906 ) ) ;
#4161 = DIRECTION ( 'NONE',  ( 0.000000000000000000, -1.000000000000000000, -0.000000000000000000 ) ) ;
#4162 = CYLINDRICAL_SURFACE ( 'NONE', #3215, 5.000000000000000888 ) ;
#4163 =( BOUNDED_SURFACE ( )  B_SPLINE_SURFACE ( 3, 1, ( 
 ( #84, #1705 ),
 ( #10312, #15940 ),
 ( #14602, #8678 ),
 ( #6008, #4380 ) ),
 .UNSPECIFIED., .F., .F., .T. ) 
 B_SPLINE_SURFACE_WITH_KNOTS ( ( 4, 4 ),
 ( 2, 2 ),
 ( 0.000000000000000000, 1.000000000000000000 ),
 ( 0.000000000000000000, 1.000000000000000000 ),
 .UNSPECIFIED. ) 
 GEOMETRIC_REPRESENTATION_ITEM ( )  RATIONAL_B_SPLINE_SURFACE ( (
 ( 1.000000000000000000, 1.000000000000000000),
 ( 0.9933953342250436691, 0.8357391271907733676),
 ( 0.9933953342250436691, 0.8357391271907733676),
 ( 1.000000000000000000, 1.000000000000000000) ) ) 
 REPRESENTATION_ITEM ( '' )  SURFACE ( )  );
#4164 = SHAPE_REPRESENTATION_RELATIONSHIP ( 'NONE' , 'NONE' ,  #9113, #10845 ) ;
#4165 = CARTESIAN_POINT ( 'NONE',  ( 1.560000000000000053, 0.000000000000000000, 2.999999999999998668 ) ) ;
#4166 = LINE ( 'NONE', #1196, #13360 ) ;
#4167 = CARTESIAN_POINT ( 'NONE',  ( 16.57778382496167424, 0.01482878558584695486, -0.001819584982831739346 ) ) ;
#4168 = DIRECTION ( 'NONE',  ( 0.000000000000000000, 1.000000000000000000, 0.000000000000000000 ) ) ;
#4169 = STYLED_ITEM ( 'NONE', ( #2162 ), #16154 ) ;
#4170 = ORIENTED_EDGE ( 'NONE', *, *, #11302, .F. ) ;
#4171 = VERTEX_POINT ( 'NONE', #3529 ) ;
#4172 = VECTOR ( 'NONE', #3531, 1000.000000000000000 ) ;
#4173 = ORIENTED_EDGE ( 'NONE', *, *, #9481, .F. ) ;
#4174 = B_SPLINE_CURVE_WITH_KNOTS ( 'NONE', 3,
 ( #6637, #9211, #12453, #15140 ),
 .UNSPECIFIED., .F., .F.,
 ( 4, 4 ),
 ( 4.873469348537302793E-16, 0.002004993803842133101 ),
 .UNSPECIFIED. ) ;
#4175 = ORIENTED_EDGE ( 'NONE', *, *, #4872, .T. ) ;
#4176 = ORIENTED_EDGE ( 'NONE', *, *, #12342, .F. ) ;
#4177 = LINE ( 'NONE', #13436, #12921 ) ;
#4178 = AXIS2_PLACEMENT_3D ( 'NONE', #17302, #8247, #4221 ) ;
#4179 = DIRECTION ( 'NONE',  ( 1.000000000000000000, 0.000000000000000000, -0.000000000000000000 ) ) ;
#4180 = B_SPLINE_CURVE_WITH_KNOTS ( 'NONE', 3,
 ( #4947, #3602, #3690, #2256, #735, #2173, #12216, #13645, #8010, #17955, #562, #10970, #12390 ),
 .UNSPECIFIED., .F., .F.,
 ( 4, 3, 3, 3, 4 ),
 ( 1.734723475976807094E-18, 0.0002299804304191486635, 0.0004599608082120272860, 0.0006467586077648025591, 0.0008336169836825982902 ),
 .UNSPECIFIED. ) ;
#4181 = LINE ( 'NONE', #12863, #9350 ) ;
#4182 = ORIENTED_EDGE ( 'NONE', *, *, #16689, .F. ) ;
#4183 = CARTESIAN_POINT ( 'NONE',  ( 3.353306896162455697, 13.88482890973696726, 1.348936822032873240 ) ) ;
#4184 = CIRCLE ( 'NONE', #1114, 3.499999999999992895 ) ;
#4185 = EDGE_CURVE ( 'NONE', #181, #5397, #17747, .T. ) ;
#4186 =( GEOMETRIC_REPRESENTATION_CONTEXT ( 3 ) GLOBAL_UNCERTAINTY_ASSIGNED_CONTEXT ( ( #2496 ) ) GLOBAL_UNIT_ASSIGNED_CONTEXT ( ( #1765, #6067, #3176 ) ) REPRESENTATION_CONTEXT ( 'NONE', 'WORKASPACE' ) );
#4187 = FACE_OUTER_BOUND ( 'NONE', #17414, .T. ) ;
#4188 = CARTESIAN_POINT ( 'NONE',  ( 2.564349062531208645, 7.499999999999999112, -15.65236830614206909 ) ) ;
#4189 = CLOSED_SHELL ( 'NONE', ( #297, #7987, #9459, #11355, #4727, #17066, #8467, #18898, #9820, #4892, #7667, #11879, #11295, #14268, #8812, #8260, #18591, #14598, #18465, #18406, #2462, #16106, #2954, #16000, #18217, #9314, #7143, #4861, #13549, #11149, #9662, #7236 ) ) ;
#4190 = CARTESIAN_POINT ( 'NONE',  ( 2.320521194583481606, -1.795798718314370213, -15.64520804578356561 ) ) ;
#4191 = B_SPLINE_CURVE_WITH_KNOTS ( 'NONE', 3,
 ( #4876, #4681, #11945, #4775 ),
 .UNSPECIFIED., .F., .F.,
 ( 4, 4 ),
 ( 4.336808689942017736E-19, 0.003005512676784827947 ),
 .UNSPECIFIED. ) ;
#4192 = CARTESIAN_POINT ( 'NONE',  ( 1.499999999999998668, 6.799999999999999822, 5.000000000000000000 ) ) ;
#4193 = CARTESIAN_POINT ( 'NONE',  ( 3.950837973638668288, 0.000000000000000000, 0.000000000000000000 ) ) ;
#4194 = CARTESIAN_POINT ( 'NONE',  ( 1.846613052777652531, -3.520031056876387954, 11.93415846513960332 ) ) ;
#4195 = ORIENTED_EDGE ( 'NONE', *, *, #5467, .F. ) ;
#4196 = ORIENTED_EDGE ( 'NONE', *, *, #14979, .F. ) ;
#4197 = CARTESIAN_POINT ( 'NONE',  ( -199.9999999999999716, 4.999999999999975131, 3.000000000000002665 ) ) ;
#4198 = VECTOR ( 'NONE', #17813, 1000.000000000000000 ) ;
#4199 = VERTEX_POINT ( 'NONE', #15095 ) ;
#4200 = ORIENTED_EDGE ( 'NONE', *, *, #5975, .F. ) ;
#4201 = CARTESIAN_POINT ( 'NONE',  ( 18.30499999999999972, 0.000000000000000000, 0.000000000000000000 ) ) ;
#4202 = ORIENTED_EDGE ( 'NONE', *, *, #15921, .F. ) ;
#4203 = CARTESIAN_POINT ( 'NONE',  ( 3.353306896162455697, 3.007732942432417289, 13.62210141459496171 ) ) ;
#4204 = CARTESIAN_POINT ( 'NONE',  ( 3.950837973638668288, 0.000000000000000000, 0.000000000000000000 ) ) ;
#4205 = CARTESIAN_POINT ( 'NONE',  ( 16.58200780006414732, 0.008650561019685807859, 0.007066318000006031885 ) ) ;
#4206 = CARTESIAN_POINT ( 'NONE',  ( 16.56753206892534891, -0.001549402974393209202, 0.009369540855502124857 ) ) ;
#4207 = VERTEX_POINT ( 'NONE', #1915 ) ;
#4208 = CARTESIAN_POINT ( 'NONE',  ( 2.123976203522053297, -10.37815841598499667, 11.67822624909921814 ) ) ;
#4209 = VECTOR ( 'NONE', #6742, 1000.000000000000227 ) ;
#4210 = CARTESIAN_POINT ( 'NONE',  ( 0.3142014840576518586, -3.879477880151352753, -13.17932813834298678 ) ) ;
#4211 = CARTESIAN_POINT ( 'NONE',  ( 3.686287386450715076E-15, -27.00000000000000000, 25.01316734529526187 ) ) ;
#4212 = CARTESIAN_POINT ( 'NONE',  ( 1.342453679581834924, 14.34050741580207067, 3.649820028552781093 ) ) ;
#4213 = CARTESIAN_POINT ( 'NONE',  ( 1.846138399168762989, 11.69739621335922308, 4.238866729160444713 ) ) ;
#4214 = EDGE_CURVE ( 'NONE', #1603, #2481, #6020, .T. ) ;
#4215 = LINE ( 'NONE', #10031, #15340 ) ;
#4216 = B_SPLINE_CURVE_WITH_KNOTS ( 'NONE', 3,
 ( #6219, #13284, #7280, #199, #10136, #13384, #11860, #302, #15960, #10329 ),
 .UNSPECIFIED., .F., .F.,
 ( 4, 3, 3, 4 ),
 ( 0.0004168119862248656667, 0.0004599608082120252802, 0.0006467586077648016917, 0.0008336169836825988323 ),
 .UNSPECIFIED. ) ;
#4217 = PRODUCT_DEFINITION_CONTEXT ( 'detailed design', #14375, 'design' ) ;
#4218 = DIRECTION ( 'NONE',  ( 1.000000000000000000, 0.000000000000000000, 0.000000000000000000 ) ) ;
#4219 = CARTESIAN_POINT ( 'NONE',  ( 2.636624412714236865, 0.000000000000000000, 0.000000000000000000 ) ) ;
#4220 = DIRECTION ( 'NONE',  ( 2.891205793294679312E-16, 1.000000000000000000, -0.000000000000000000 ) ) ;
#4222 = EDGE_LOOP ( 'NONE', ( #17056, #11964, #9426, #8154, #7583 ) ) ;
#4221 = DIRECTION ( 'NONE',  ( 0.000000000000000000, 0.000000000000000000, 1.000000000000000000 ) ) ;
#4223 = DIRECTION ( 'NONE',  ( -0.7561779333270775005, -0.6106991889125072959, 0.2350349629540161855 ) ) ;
#4224 = AXIS2_PLACEMENT_3D ( 'NONE', #12507, #6693, #13494 ) ;
#4225 = DIRECTION ( 'NONE',  ( 0.000000000000000000, 0.000000000000000000, -1.000000000000000000 ) ) ;
#4226 = ORIENTED_EDGE ( 'NONE', *, *, #17570, .F. ) ;
#4227 = CARTESIAN_POINT ( 'NONE',  ( 2.705023505549863039, -12.36217802824809020, 4.909285963184022883 ) ) ;
#4228 = CARTESIAN_POINT ( 'NONE',  ( 2.636624412715362631, -15.80357026013197519, 2.862162146984090327 ) ) ;
#4229 = ORIENTED_EDGE ( 'NONE', *, *, #11914, .F. ) ;
#4230 = DIRECTION ( 'NONE',  ( -1.000000000000000000, -0.000000000000000000, -0.000000000000000000 ) ) ;
#4231 = CARTESIAN_POINT ( 'NONE',  ( 0.4862570985993252548, -3.580942890621766406, 13.44146924561379741 ) ) ;
#4232 = CARTESIAN_POINT ( 'NONE',  ( 0.3307726912345235748, -3.680742887039399669, 13.25328329128664606 ) ) ;
#4233 = CARTESIAN_POINT ( 'NONE',  ( 0.4862570985993252548, 3.580942890621670482, 13.44146924561382583 ) ) ;
#4234 = CARTESIAN_POINT ( 'NONE',  ( -30.00000000000000355, -12.50000000000000178, 0.000000000000000000 ) ) ;
#4235 = ADVANCED_FACE ( 'NONE', ( #9364 ), #11851, .T. ) ;
#4236 = ADVANCED_FACE ( 'NONE', ( #2013 ), #3354, .F. ) ;
#4237 = ORIENTED_EDGE ( 'NONE', *, *, #4371, .F. ) ;
#4238 = EDGE_CURVE ( 'NONE', #14839, #12842, #11714, .T. ) ;
#4239 = ITEM_DEFINED_TRANSFORMATION ( 'NONE', 'NONE', #12717,  #2030 ) ;
#4240 = FACE_OUTER_BOUND ( 'NONE', #18688, .T. ) ;
#4241 = CARTESIAN_POINT ( 'NONE',  ( 0.4754618798421167414, 8.775436892861268490, -10.80499583390503560 ) ) ;
#4242 = DIRECTION ( 'NONE',  ( 0.7635533937278216055, 0.02138673900302332995, -0.6453904417649386493 ) ) ;
#4243 = CARTESIAN_POINT ( 'NONE',  ( 2.123976203522053297, 11.67822624909925544, 10.37815841598495936 ) ) ;
#4244 = CARTESIAN_POINT ( 'NONE',  ( 1.846138399168762101, -12.43476674860266229, -0.4167076046096845898 ) ) ;
#4245 = ORIENTED_EDGE ( 'NONE', *, *, #7685, .T. ) ;
#4246 = CARTESIAN_POINT ( 'NONE',  ( -30.00000000000000355, -12.50000000000000178, 6.500000000000000888 ) ) ;
#4247 = CARTESIAN_POINT ( 'NONE',  ( 0.4754618798421167414, -5.007009103465340338, 12.98792082933642966 ) ) ;
#4248 = VERTEX_POINT ( 'NONE', #10411 ) ;
#4249 = ORIENTED_EDGE ( 'NONE', *, *, #9691, .T. ) ;
#4250 = CARTESIAN_POINT ( 'NONE',  ( 0.4862570985993235340, 8.769551628660735787, 10.79774104611376373 ) ) ;
#4251 = ORIENTED_EDGE ( 'NONE', *, *, #17943, .T. ) ;
#4252 = CARTESIAN_POINT ( 'NONE',  ( 0.3058872367615226295, 4.821066432589507400, -12.87003593440623206 ) ) ;
#4253 = VECTOR ( 'NONE', #8146, 1000.000000000000114 ) ;
#4254 = ORIENTED_EDGE ( 'NONE', *, *, #4447, .T. ) ;
#4255 = DIRECTION ( 'NONE',  ( -0.000000000000000000, -0.000000000000000000, 1.000000000000000000 ) ) ;
#4256 = CARTESIAN_POINT ( 'NONE',  ( 1.846138399168762101, -10.30487220521565028, -6.971848976711123136 ) ) ;
#4257 = VECTOR ( 'NONE', #3309, 1000.000000000000000 ) ;
#4258 = CARTESIAN_POINT ( 'NONE',  ( 0.3151926232592475174, -8.013596737356467159, 11.16039997398650918 ) ) ;
#4259 = CARTESIAN_POINT ( 'NONE',  ( 0.3095370825347233956, -7.700448427571951804, 11.38092634279625948 ) ) ;
#4260 = DIRECTION ( 'NONE',  ( 0.000000000000000000, 0.000000000000000000, 1.000000000000000000 ) ) ;
#4261 = CARTESIAN_POINT ( 'NONE',  ( 0.4385251269669980800, -3.577373010348622540, -13.39302348765812312 ) ) ;
#4262 = CARTESIAN_POINT ( 'NONE',  ( 0.4385251269669942498, -10.76637725024245462, -8.732456510146192841 ) ) ;
#4263 = EDGE_CURVE ( 'NONE', #10243, #9140, #9077, .T. ) ;
#4264 = AXIS2_PLACEMENT_3D ( 'NONE', #8501, #1227, #7165 ) ;
#4265 = CARTESIAN_POINT ( 'NONE',  ( 0.3170788640506440603, 11.20690911610915208, -7.952793437297452250 ) ) ;
#4266 = CARTESIAN_POINT ( 'NONE',  ( 2.369999999999999662, 0.000000000000000000, 0.000000000000000000 ) ) ;
#4267 = ORIENTED_EDGE ( 'NONE', *, *, #18778, .T. ) ;
#4268 = VERTEX_POINT ( 'NONE', #14805 ) ;
#4269 = ORIENTED_EDGE ( 'NONE', *, *, #14784, .F. ) ;
#4270 = ORIENTED_EDGE ( 'NONE', *, *, #1806, .F. ) ;
#4271 = ORIENTED_EDGE ( 'NONE', *, *, #10896, .F. ) ;
#4272 = CARTESIAN_POINT ( 'NONE',  ( 4.176146106109656457E-15, -16.60000000000000142, 29.01316734529526187 ) ) ;
#4273 = LINE ( 'NONE', #5879, #2006 ) ;
#4274 = CARTESIAN_POINT ( 'NONE',  ( 2.636624412714242194, 14.46769361191244485, 6.973567714906650394 ) ) ;
#4275 = EDGE_LOOP ( 'NONE', ( #9085, #15313, #12875, #17450 ) ) ;
#4276 = FACE_BOUND ( 'NONE', #5652, .T. ) ;
#4277 = CARTESIAN_POINT ( 'NONE',  ( 0.3137051932979775248, 0.4596302728639756197, 13.73004976592202198 ) ) ;
#4278 = CARTESIAN_POINT ( 'NONE',  ( 4.482738663876791207, 5.389345431477718940, -11.99999999527195627 ) ) ;
#4279 = LINE ( 'NONE', #3009, #1876 ) ;
#4280 = CARTESIAN_POINT ( 'NONE',  ( 0.3137051932979792457, -10.83767969834809008, 8.442169467526815296 ) ) ;
#4281 = ADVANCED_FACE ( 'NONE', ( #1714 ), #5306, .F. ) ;
#4282 = CARTESIAN_POINT ( 'NONE',  ( 1.959212340397942231, 12.12975361829680310, -3.239239832448903122 ) ) ;
#4283 = CARTESIAN_POINT ( 'NONE',  ( 1.847372867223028070, 3.744745203533978106, 11.86627781945709792 ) ) ;
#4284 = ADVANCED_FACE ( 'NONE', ( #483 ), #6310, .T. ) ;
#4285 = CARTESIAN_POINT ( 'NONE',  ( 0.3939875929385661668, 4.930599594904554017, 12.90850834464102270 ) ) ;
#4286 = CARTESIAN_POINT ( 'NONE',  ( 2.002547531651519996, 4.532360870844494016, -11.75462648437097180 ) ) ;
#4287 = EDGE_LOOP ( 'NONE', ( #4480, #15707, #17179, #10381 ) ) ;
#4288 = ORIENTED_EDGE ( 'NONE', *, *, #1459, .F. ) ;
#4289 = AXIS2_PLACEMENT_3D ( 'NONE', #4211, #5813, #9832 ) ;
#4290 = ORIENTED_EDGE ( 'NONE', *, *, #7556, .T. ) ;
#4291 = VERTEX_POINT ( 'NONE', #18514 ) ;
#4292 = EDGE_CURVE ( 'NONE', #17548, #14697, #14995, .T. ) ;
#4293 = ORIENTED_EDGE ( 'NONE', *, *, #388, .T. ) ;
#4294 = CARTESIAN_POINT ( 'NONE',  ( 0.4385251269669980800, -3.577373010348622540, -13.39302348765812312 ) ) ;
#4295 = DIRECTION ( 'NONE',  ( -0.4246593920385850485, -0.1376957914266803973, 0.8948208031649685923 ) ) ;
#4296 = CARTESIAN_POINT ( 'NONE',  ( 3.950837973638668288, 0.000000000000000000, 0.000000000000000000 ) ) ;
#4297 = CYLINDRICAL_SURFACE ( 'NONE', #1371, 5.000000000000000000 ) ;
#4298 = VERTEX_POINT ( 'NONE', #2368 ) ;
#4299 = FACE_OUTER_BOUND ( 'NONE', #14872, .T. ) ;
#4300 = DIRECTION ( 'NONE',  ( -0.5000000000000042188, 1.060575238724903710E-16, -0.8660254037844361541 ) ) ;
#4301 = DIRECTION ( 'NONE',  ( -0.000000000000000000, -0.000000000000000000, 1.000000000000000000 ) ) ;
#4302 = DIRECTION ( 'NONE',  ( 0.000000000000000000, 0.000000000000000000, -1.000000000000000000 ) ) ;
#4303 = DIRECTION ( 'NONE',  ( 0.000000000000000000, 0.000000000000000000, 1.000000000000000000 ) ) ;
#4304 = CARTESIAN_POINT ( 'NONE',  ( 1.846138399168762101, -12.43476674860266229, -0.4167076046096845898 ) ) ;
#4305 = CARTESIAN_POINT ( 'NONE',  ( -2.854984224814739692E-15, 4.485238902526780435E-17, 8.437203105296061878 ) ) ;
#4306 = LINE ( 'NONE', #5817, #2830 ) ;
#4307 = ORIENTED_EDGE ( 'NONE', *, *, #9073, .F. ) ;
#4308 = AXIS2_PLACEMENT_3D ( 'NONE', #10712, #15203, #6596 ) ;
#4309 = CARTESIAN_POINT ( 'NONE',  ( 1.977436885025838142, -14.12046670317529440, -6.153171729168441573 ) ) ;
#4311 = EDGE_LOOP ( 'NONE', ( #17254, #12858, #4692, #15941 ) ) ;
#4310 = CARTESIAN_POINT ( 'NONE',  ( 2.002547531651519996, 9.778737580845815458, -7.942910686618064986 ) ) ;
#4312 = EDGE_CURVE ( 'NONE', #11465, #5954, #2275, .T. ) ;
#4313 = LINE ( 'NONE', #10138, #11826 ) ;
#4314 = CARTESIAN_POINT ( 'NONE',  ( -2.179449471770337432, -4.500000000000000000, -3.000000000000000000 ) ) ;
#4315 = EDGE_CURVE ( 'NONE', #5180, #11553, #2235, .T. ) ;
#4316 = ORIENTED_EDGE ( 'NONE', *, *, #374, .T. ) ;
#4317 = CARTESIAN_POINT ( 'NONE',  ( 1.846955891736115740, 10.21904526726846640, 7.098901504650394934 ) ) ;
#4318 = PRODUCT_DEFINITION_SHAPE ( 'NONE', 'NONE',  #18908 ) ;
#4319 = CARTESIAN_POINT ( 'NONE',  ( 1.876333640634852307, -7.500000000000000888, -15.16052078710814932 ) ) ;
#4320 = ORIENTED_EDGE ( 'NONE', *, *, #272, .T. ) ;
#4321 = CARTESIAN_POINT ( 'NONE',  ( 2.636624412714237309, 14.14563173255211126, 7.605649742762011556 ) ) ;
#4322 = DIRECTION ( 'NONE',  ( -1.000000000000000000, 0.000000000000000000, 0.000000000000000000 ) ) ;
#4323 = AXIS2_PLACEMENT_3D ( 'NONE', #16567, #9108, #3361 ) ;
#4324 = CARTESIAN_POINT ( 'NONE',  ( 0.3132642857406524040, 3.740125687984731773, 13.21852905223340535 ) ) ;
#4325 = DIRECTION ( 'NONE',  ( -1.000000000000000000, 0.000000000000000000, -0.000000000000000000 ) ) ;
#4326 = VERTEX_POINT ( 'NONE', #5422 ) ;
#4327 = DIRECTION ( 'NONE',  ( 0.000000000000000000, 0.000000000000000000, 1.000000000000000000 ) ) ;
#4328 = CARTESIAN_POINT ( 'NONE',  ( 16.58200780006414732, 0.01115192838421568376, 0.0006320991582350033409 ) ) ;
#4329 = CARTESIAN_POINT ( 'NONE',  ( 1.846138399168762101, 0.4167076046095548603, 12.43476674860266762 ) ) ;
#4330 = FACE_OUTER_BOUND ( 'NONE', #13068, .T. ) ;
#4331 = CARTESIAN_POINT ( 'NONE',  ( 3.950837973638676281, -6.888253895133199300, -12.81214529934982949 ) ) ;
#4332 = ORIENTED_EDGE ( 'NONE', *, *, #3767, .T. ) ;
#4333 = DIRECTION ( 'NONE',  ( -0.000000000000000000, -1.000000000000000000, -0.000000000000000000 ) ) ;
#4334 = CARTESIAN_POINT ( 'NONE',  ( 16.56679352167444819, -0.004277682826583350043, -0.008252760440870175046 ) ) ;
#4335 = EDGE_LOOP ( 'NONE', ( #11113, #10310, #18052, #4606 ) ) ;
#4336 = EDGE_CURVE ( 'NONE', #3103, #14004, #7947, .T. ) ;
#4337 = EDGE_CURVE ( 'NONE', #3494, #9678, #13853, .T. ) ;
#4338 = EDGE_CURVE ( 'NONE', #15500, #4964, #14033, .T. ) ;
#4339 = ORIENTED_EDGE ( 'NONE', *, *, #10048, .F. ) ;
#4340 = CARTESIAN_POINT ( 'NONE',  ( -194.9999999999999716, 4.999999999999973355, 3.000000000000002665 ) ) ;
#4341 = VERTEX_POINT ( 'NONE', #8301 ) ;
#4342 = CARTESIAN_POINT ( 'NONE',  ( 0.3058872367615226295, -13.72992299905059355, -0.6080468242582393046 ) ) ;
#4343 = VECTOR ( 'NONE', #14895, 1000.000000000000114 ) ;
#4344 = VERTEX_POINT ( 'NONE', #6778 ) ;
#4345 = DIRECTION ( 'NONE',  ( -1.000000000000000000, 0.000000000000000000, 0.000000000000000000 ) ) ;
#4346 = CARTESIAN_POINT ( 'NONE',  ( 16.56753206892534891, 0.009389754735542247058, 0.001421777558675981282 ) ) ;
#4347 = DIRECTION ( 'NONE',  ( -1.000000000000000000, -0.000000000000000000, -0.000000000000000000 ) ) ;
#4348 = CARTESIAN_POINT ( 'NONE',  ( 2.320521194584331148, 11.60169518685982304, -10.64885423995325198 ) ) ;
#4349 = EDGE_CURVE ( 'NONE', #12310, #7136, #17494, .T. ) ;
#4350 = SURFACE_STYLE_FILL_AREA ( #3283 ) ;
#4351 = CARTESIAN_POINT ( 'NONE',  ( 2.747332970342022840, -16.17136872824900351, 2.409922051470623661 ) ) ;
#4352 = CARTESIAN_POINT ( 'NONE',  ( 1.499999999999998668, 6.799999999999999822, 7.000000000000000000 ) ) ;
#4353 = CARTESIAN_POINT ( 'NONE',  ( 16.57778382496167424, 0.01466529584256671612, -0.002851818597093459199 ) ) ;
#4354 = CARTESIAN_POINT ( 'NONE',  ( 0.3137051932979757485, 13.73004976592202020, -0.4596302728640235258 ) ) ;
#4355 = EDGE_LOOP ( 'NONE', ( #2045, #6769, #17331, #4147 ) ) ;
#4356 = ORIENTED_EDGE ( 'NONE', *, *, #10209, .T. ) ;
#4357 = AXIS2_PLACEMENT_3D ( 'NONE', #10857, #10567, #4735 ) ;
#4358 = EDGE_LOOP ( 'NONE', ( #3000, #9279, #329, #5658 ) ) ;
#4359 = ORIENTED_EDGE ( 'NONE', *, *, #13647, .T. ) ;
#4360 = B_SPLINE_CURVE_WITH_KNOTS ( 'NONE', 3,
 ( #8863, #1410, #10302, #1697, #11641, #12025 ),
 .UNSPECIFIED., .F., .F.,
 ( 4, 2, 4 ),
 ( 4.225718824587268470E-17, 0.0002014099069817298145, 0.0004028198139634173993 ),
 .UNSPECIFIED. ) ;
#4361 = VERTEX_POINT ( 'NONE', #13842 ) ;
#4362 = CARTESIAN_POINT ( 'NONE',  ( 1.846822687350018644, 4.121816957446363894, -11.74004266906800353 ) ) ;
#4363 = ADVANCED_FACE ( 'NONE', ( #18418 ), #13123, .F. ) ;
#4364 = CARTESIAN_POINT ( 'NONE',  ( 20.00000000000000000, 7.499999999999999112, -16.99999999999999645 ) ) ;
#4365 = ORIENTED_EDGE ( 'NONE', *, *, #8665, .F. ) ;
#4366 = CARTESIAN_POINT ( 'NONE',  ( 2.636624412714763555, 6.973567714907159321, 14.46769361191226722 ) ) ;
#4367 = CARTESIAN_POINT ( 'NONE',  ( 1.342453679581834924, -0.9602753779831757486, 14.76648944001038899 ) ) ;
#4368 = DIRECTION ( 'NONE',  ( 1.000000000000000000, 0.000000000000000000, 0.000000000000000000 ) ) ;
#4369 = CARTESIAN_POINT ( 'NONE',  ( 3.950837973638668288, 14.41405733518061538, -1.958075594453841273 ) ) ;
#4370 = CARTESIAN_POINT ( 'NONE',  ( 0.3137051932979792457, -11.37800749014136592, 7.698472063774431717 ) ) ;
#4371 = EDGE_CURVE ( 'NONE', #3595, #10401, #15282, .T. ) ;
#4372 = CARTESIAN_POINT ( 'NONE',  ( 1.846138399168762101, 0.4167076046097279440, -12.43476674860266051 ) ) ;
#4373 = CARTESIAN_POINT ( 'NONE',  ( 0.3095370825347233956, -11.38092634279623105, -7.700448427571997101 ) ) ;
#4374 = CARTESIAN_POINT ( 'NONE',  ( 15.00000000000000711, -14.99999999999999645, 3.000000000000000000 ) ) ;
#4375 = SPHERICAL_SURFACE ( 'NONE', #8750, 5.000000000000000000 ) ;
#4376 = VERTEX_POINT ( 'NONE', #758 ) ;
#4377 = ORIENTED_EDGE ( 'NONE', *, *, #5439, .T. ) ;
#4378 = ORIENTED_EDGE ( 'NONE', *, *, #1372, .F. ) ;
#4379 = VERTEX_POINT ( 'NONE', #6591 ) ;
#4380 = CARTESIAN_POINT ( 'NONE',  ( 0.4754618798421162973, 13.89949764182682657, 0.7484603771384912285 ) ) ;
#4381 = VECTOR ( 'NONE', #10253, 1000.000000000000000 ) ;
#4382 = ORIENTED_EDGE ( 'NONE', *, *, #4336, .T. ) ;
#4383 = DIRECTION ( 'NONE',  ( 1.540743955509788340E-33, 1.000000000000000000, 2.533398541561209262E-17 ) ) ;
#4384 = AXIS2_PLACEMENT_3D ( 'NONE', #9240, #4564, #1985 ) ;
#4385 = DIRECTION ( 'NONE',  ( -0.000000000000000000, -0.000000000000000000, 1.000000000000000000 ) ) ;
#4386 = DIRECTION ( 'NONE',  ( 0.000000000000000000, 1.000000000000000000, 0.000000000000000000 ) ) ;
#4387 = ORIENTED_EDGE ( 'NONE', *, *, #5486, .F. ) ;
#4388 = DIRECTION ( 'NONE',  ( 1.000000000000000000, 0.000000000000000000, 0.000000000000000000 ) ) ;
#4389 = CYLINDRICAL_SURFACE ( 'NONE', #6098, 5.000000000000000888 ) ;
#4390 = ADVANCED_FACE ( 'NONE', ( #15367 ), #1284, .F. ) ;
#4391 = CARTESIAN_POINT ( 'NONE',  ( 1.846822687350018422, 11.74004266906804617, 4.121816957446238661 ) ) ;
#4392 = CARTESIAN_POINT ( 'NONE',  ( 1.918918678667044908, -6.832809802519085096, 10.48466773720559608 ) ) ;
#4393 = ADVANCED_FACE ( 'NONE', ( #14494 ), #10504, .T. ) ;
#4394 = DIRECTION ( 'NONE',  ( -1.000000000000000000, -0.000000000000000000, -0.000000000000000000 ) ) ;
#4395 = ORIENTED_EDGE ( 'NONE', *, *, #4153, .T. ) ;
#4396 = VECTOR ( 'NONE', #6434, 1000.000000000000000 ) ;
#4397 = CARTESIAN_POINT ( 'NONE',  ( 3.512766787570769544, 10.87507422923904166, -10.40533104696121214 ) ) ;
#4399 = ORIENTED_EDGE ( 'NONE', *, *, #3927, .T. ) ;
#4398 = CARTESIAN_POINT ( 'NONE',  ( 0.000000000000000000, 0.000000000000000000, 2.499999999999999556 ) ) ;
#4400 = CARTESIAN_POINT ( 'NONE',  ( 0.3058872367615230181, 3.664492643742949252, -13.24582953854921463 ) ) ;
#4401 = ORIENTED_EDGE ( 'NONE', *, *, #14384, .T. ) ;
#4402 = LINE ( 'NONE', #10237, #2478 ) ;
#4403 = ORIENTED_EDGE ( 'NONE', *, *, #1748, .T. ) ;
#4404 = CARTESIAN_POINT ( 'NONE',  ( 0.3137051932979775248, -0.4596302728638797519, -13.73004976592202553 ) ) ;
#4405 = CARTESIAN_POINT ( 'NONE',  ( 3.382406833283068348, -7.500000000000000888, -16.15212677409162012 ) ) ;
#4406 = VERTEX_POINT ( 'NONE', #7145 ) ;
#4407 = CARTESIAN_POINT ( 'NONE',  ( 16.56822296793089322, -0.009847136207496290372, -0.002414375228568220195 ) ) ;
#4408 = AXIS2_PLACEMENT_3D ( 'NONE', #12984, #11657, #8506 ) ;
#4409 = CARTESIAN_POINT ( 'NONE',  ( 5.000000000000000000, 20.00000000000000000, 8.000000000000000000 ) ) ;
#4410 = CARTESIAN_POINT ( 'NONE',  ( 0.3145729642390375225, -3.952965287571204023, 13.15786090015082799 ) ) ;
#4411 = CARTESIAN_POINT ( 'NONE',  ( 0.3939822652208163078, 3.598529276937260324, 13.34132036472938410 ) ) ;
#4412 = TOROIDAL_SURFACE ( 'NONE', #16003, 3.499999999999994671, 0.5000000000000000000 ) ;
#4413 = EDGE_CURVE ( 'NONE', #3962, #14617, #15736, .T. ) ;
#4414 = VECTOR ( 'NONE', #3982, 1000.000000000000000 ) ;
#4415 = ITEM_DEFINED_TRANSFORMATION ( 'NONE', 'NONE', #14252,  #2030 ) ;
#4416 = CARTESIAN_POINT ( 'NONE',  ( 16.56782317627811096, -0.006045301465876417625, 0.007739510688079494216 ) ) ;
#4417 = EDGE_CURVE ( 'NONE', #6836, #15610, #14148, .T. ) ;
#4418 = CARTESIAN_POINT ( 'NONE',  ( 3.353306896162455697, -13.62210141459498125, 3.007732942432364442 ) ) ;
#4419 = CARTESIAN_POINT ( 'NONE',  ( 16.56782317627811096, -0.002708056627497679603, 0.009439921864426459655 ) ) ;
#4420 = CARTESIAN_POINT ( 'NONE',  ( 5.000000000000000000, 20.00000000000000000, 4.000000000000000000 ) ) ;
#4421 = DIRECTION ( 'NONE',  ( 0.000000000000000000, 0.000000000000000000, -1.000000000000000000 ) ) ;
#4422 = VECTOR ( 'NONE', #982, 1000.000000000000114 ) ;
#4423 = ORIENTED_EDGE ( 'NONE', *, *, #10269, .T. ) ;
#4424 = CARTESIAN_POINT ( 'NONE',  ( 0.3145734862173242830, 11.29227530924457312, -7.825584895511399353 ) ) ;
#4425 = CARTESIAN_POINT ( 'NONE',  ( 0.3170788640506441158, -13.02120094575831288, 4.392045232375760833 ) ) ;
#4426 = AXIS2_PLACEMENT_3D ( 'NONE', #13422, #43, #4639 ) ;
#4427 = ORIENTED_EDGE ( 'NONE', *, *, #9427, .T. ) ;
#4428 = AXIS2_PLACEMENT_3D ( 'NONE', #4750, #3398, #9235 ) ;
#4429 = EDGE_LOOP ( 'NONE', ( #11404, #253, #4913, #370 ) ) ;
#4430 = CARTESIAN_POINT ( 'NONE',  ( 0.3307726912345191894, -4.812300915532890855, -12.88561780039863436 ) ) ;
#4431 = ORIENTED_EDGE ( 'NONE', *, *, #16809, .T. ) ;
#4432 = CARTESIAN_POINT ( 'NONE',  ( -194.9999999999999716, -5.000000000000024869, 6.000000000000000000 ) ) ;
#4433 = EDGE_LOOP ( 'NONE', ( #5874, #3791, #16540, #6204 ) ) ;
#4434 = CARTESIAN_POINT ( 'NONE',  ( 3.377929128793398128, 7.136734442941011558, -12.02809354424093691 ) ) ;
#4435 = CARTESIAN_POINT ( 'NONE',  ( 2.747332970342022840, 11.45495994260717865, 11.66639548242811486 ) ) ;
#4436 = DIRECTION ( 'NONE',  ( -1.000000000000000000, -0.000000000000000000, -0.000000000000000000 ) ) ;
#4437 =( BOUNDED_SURFACE ( )  B_SPLINE_SURFACE ( 3, 1, ( 
 ( #1133, #15473 ),
 ( #8045, #18428 ),
 ( #2288, #11368 ),
 ( #16910, #12511 ) ),
 .UNSPECIFIED., .F., .F., .T. ) 
 B_SPLINE_SURFACE_WITH_KNOTS ( ( 4, 4 ),
 ( 2, 2 ),
 ( 0.000000000000000000, 1.000000000000000000 ),
 ( 0.000000000000000000, 1.000000000000000000 ),
 .UNSPECIFIED. ) 
 GEOMETRIC_REPRESENTATION_ITEM ( )  RATIONAL_B_SPLINE_SURFACE ( (
 ( 1.000000000000000000, 1.000000000000000000),
 ( 0.9933953342250438912, 0.8357391271907739227),
 ( 0.9933953342250438912, 0.8357391271907739227),
 ( 1.000000000000000000, 1.000000000000000000) ) ) 
 REPRESENTATION_ITEM ( '' )  SURFACE ( )  );
#4438 = CARTESIAN_POINT ( 'NONE',  ( 0.3151926232592501265, 4.318679262939624230, 13.04305446098357635 ) ) ;
#4439 = UNCERTAINTY_MEASURE_WITH_UNIT (LENGTH_MEASURE( 1.000000000000000082E-05 ), #6432, 'distance_accuracy_value', 'NONE');
#4440 = CIRCLE ( 'NONE', #9931, 1.000000000000000000 ) ;
#4441 = CARTESIAN_POINT ( 'NONE',  ( -4.999999999999995559, -30.00000000000000000, 31.00000000000000000 ) ) ;
#4442 = FACE_OUTER_BOUND ( 'NONE', #11414, .T. ) ;
#4443 = AXIS2_PLACEMENT_3D ( 'NONE', #11088, #12592, #9464 ) ;
#4444 = PRESENTATION_STYLE_ASSIGNMENT (( #7417 ) ) ;
#4445 = EDGE_CURVE ( 'NONE', #5155, #5851, #18429, .T. ) ;
#4446 = CARTESIAN_POINT ( 'NONE',  ( 0.000000000000000000, 6.799999999999999822, -1.500000000000000000 ) ) ;
#4447 = EDGE_CURVE ( 'NONE', #15917, #5851, #15653, .T. ) ;
#4448 = CARTESIAN_POINT ( 'NONE',  ( -26.50000000000001066, -12.50000000000000178, 6.500000000000000888 ) ) ;
#4449 = CARTESIAN_POINT ( 'NONE',  ( 16.57210152137263393, 0.01214401161737518019, -0.008007331252332923130 ) ) ;
#4450 = CARTESIAN_POINT ( 'NONE',  ( -20.00000000000000000, 0.000000000000000000, -22.00000000000000000 ) ) ;
#4451 = ORIENTED_EDGE ( 'NONE', *, *, #3045, .T. ) ;
#4452 = CARTESIAN_POINT ( 'NONE',  ( 16.57778382496167424, -0.01306626476309294925, 0.007244066302946726259 ) ) ;
#4453 = ORIENTED_EDGE ( 'NONE', *, *, #2566, .F. ) ;
#4454 = EDGE_LOOP ( 'NONE', ( #8547, #16780, #7578 ) ) ;
#4455 = VERTEX_POINT ( 'NONE', #4277 ) ;
#4456 = CIRCLE ( 'NONE', #1088, 5.000000000000004441 ) ;
#4457 = VERTEX_POINT ( 'NONE', #9906 ) ;
#4458 = AXIS2_PLACEMENT_3D ( 'NONE', #7767, #17893, #2027 ) ;
#4459 = CARTESIAN_POINT ( 'NONE',  ( 3.377929128793394575, 5.536064832134161229, 12.84367544717937548 ) ) ;
#4460 = FACE_OUTER_BOUND ( 'NONE', #573, .T. ) ;
#4461 = DIRECTION ( 'NONE',  ( -0.7635533937278216055, -0.02138673900301441000, -0.6453904417649389824 ) ) ;
#4462 = ORIENTED_EDGE ( 'NONE', *, *, #9719, .T. ) ;
#4463 = LINE ( 'NONE', #4753, #12953 ) ;
#4464 = CARTESIAN_POINT ( 'NONE',  ( 0.4384471787762819206, -11.63197976518323173, -7.540925784514680430 ) ) ;
#4465 = CARTESIAN_POINT ( 'NONE',  ( 4.755015822784811164, -4.336808689942017736E-16, 0.000000000000000000 ) ) ;
#4466 = DIRECTION ( 'NONE',  ( -1.601283208593975514E-16, 1.000000000000000000, -0.000000000000000000 ) ) ;
#4467 = CARTESIAN_POINT ( 'NONE',  ( 3.512766787570746452, -10.40533104696126898, -10.87507422923902034 ) ) ;
#4468 = EDGE_CURVE ( 'NONE', #3512, #17476, #7010, .T. ) ;
#4469 = EDGE_CURVE ( 'NONE', #11211, #3961, #2726, .T. ) ;
#4470 = DIRECTION ( 'NONE',  ( 0.000000000000000000, 0.000000000000000000, -1.000000000000000000 ) ) ;
#4471 = LINE ( 'NONE', #5891, #18430 ) ;
#4472 = EDGE_CURVE ( 'NONE', #6482, #13762, #11542, .T. ) ;
#4473 = PLANE ( 'NONE',  #15293 ) ;
#4474 = MECHANICAL_DESIGN_GEOMETRIC_PRESENTATION_REPRESENTATION (  '', ( #15448 ), #15756 ) ;
#4475 = CARTESIAN_POINT ( 'NONE',  ( 1.847412631396501803, 7.278870946904251404, 10.09191835241965407 ) ) ;
#4476 = ORIENTED_EDGE ( 'NONE', *, *, #4714, .F. ) ;
#4477 = PRODUCT ( 'socket button head screw_iso_ISO 7380 - M5 x 16 - 16C', 'socket button head screw_iso_ISO 7380 - M5 x 16 - 16C', '', ( #18110 ) ) ;
#4478 = SHAPE_REPRESENTATION ( 'socket button head screw_iso_ISO 7380 - M5 x 16 - 16C', ( #2030 ), #16378 ) ;
#4479 =( BOUNDED_SURFACE ( )  B_SPLINE_SURFACE ( 3, 1, ( 
 ( #13564, #14998 ),
 ( #485, #12147 ),
 ( #16545, #7567 ),
 ( #10618, #11853 ) ),
 .UNSPECIFIED., .F., .F., .T. ) 
 B_SPLINE_SURFACE_WITH_KNOTS ( ( 4, 4 ),
 ( 2, 2 ),
 ( 0.000000000000000000, 1.000000000000000000 ),
 ( 0.000000000000000000, 1.000000000000000000 ),
 .UNSPECIFIED. ) 
 GEOMETRIC_REPRESENTATION_ITEM ( )  RATIONAL_B_SPLINE_SURFACE ( (
 ( 1.000000000000000000, 1.000000000000000000),
 ( 0.7792777138730158093, 0.9689936506012928330),
 ( 0.7792777138730158093, 0.9689936506012928330),
 ( 1.000000000000000000, 1.000000000000000000) ) ) 
 REPRESENTATION_ITEM ( '' )  SURFACE ( )  );
#4480 = ORIENTED_EDGE ( 'NONE', *, *, #8314, .F. ) ;
#4481 = ORIENTED_EDGE ( 'NONE', *, *, #2994, .T. ) ;
#4482 = CIRCLE ( 'NONE', #6924, 5.000000000000004441 ) ;
#4483 = ORIENTED_EDGE ( 'NONE', *, *, #2000, .T. ) ;
#4484 = FACE_OUTER_BOUND ( 'NONE', #9467, .T. ) ;
#4485 = VECTOR ( 'NONE', #6481, 1000.000000000000000 ) ;
#4486 = AXIS2_PLACEMENT_3D ( 'NONE', #6509, #12330, #12156 ) ;
#4487 = ORIENTED_EDGE ( 'NONE', *, *, #14077, .T. ) ;
#4488 = CARTESIAN_POINT ( 'NONE',  ( -1.500000000000000888, 4.769696007084728073, 7.000000000000000000 ) ) ;
#4489 = CARTESIAN_POINT ( 'NONE',  ( 2.636624412715093513, -14.14563173255330142, 7.605649742761597665 ) ) ;
#4490 = CARTESIAN_POINT ( 'NONE',  ( 0.4754618798421167414, 12.98792082933644743, 5.007009103465293265 ) ) ;
#4491 =( GEOMETRIC_REPRESENTATION_CONTEXT ( 3 ) GLOBAL_UNCERTAINTY_ASSIGNED_CONTEXT ( ( #12117 ) ) GLOBAL_UNIT_ASSIGNED_CONTEXT ( ( #10598, #17764, #1800 ) ) REPRESENTATION_CONTEXT ( 'NONE', 'WORKASPACE' ) );
#4492 = FACE_OUTER_BOUND ( 'NONE', #14439, .T. ) ;
#4493 = ORIENTED_EDGE ( 'NONE', *, *, #3206, .T. ) ;
#4494 = DIRECTION ( 'NONE',  ( 0.000000000000000000, -1.224646799147353207E-16, 1.000000000000000000 ) ) ;
#4495 = AXIS2_PLACEMENT_3D ( 'NONE', #2684, #8620, #11402 ) ;
#4496 = CIRCLE ( 'NONE', #1123, 5.000000000000000888 ) ;
#4497 = CARTESIAN_POINT ( 'NONE',  ( 0.3150692679895970572, -4.099798979280757649, -13.11337225490256664 ) ) ;
#4498 = CARTESIAN_POINT ( 'NONE',  ( -199.9999999999999716, -10.00000000000002665, 6.000000000000000000 ) ) ;
#4499 = CARTESIAN_POINT ( 'NONE',  ( 0.3137051932979792457, 8.442169467527008919, -10.83767969834794087 ) ) ;
#4500 = AXIS2_PLACEMENT_3D ( 'NONE', #4246, #8631, #2602 ) ;
#4501 = VECTOR ( 'NONE', #880, 1000.000000000000000 ) ;
#4502 = CARTESIAN_POINT ( 'NONE',  ( 3.950837973638677170, 1.958075594453790869, 14.41405733518061538 ) ) ;
#4503 = ORIENTED_EDGE ( 'NONE', *, *, #6801, .F. ) ;
#4504 = EDGE_CURVE ( 'NONE', #7817, #9425, #8571, .T. ) ;
#4505 = CARTESIAN_POINT ( 'NONE',  ( -27.32408120756002035, 20.00000000000000000, 3.000000000000000000 ) ) ;
#4507 = VERTEX_POINT ( 'NONE', #12866 ) ;
#4506 = CARTESIAN_POINT ( 'NONE',  ( 0.3145729642390401870, 0.3065092323351212289, 13.73540280162740501 ) ) ;
#4508 = FACE_OUTER_BOUND ( 'NONE', #18140, .T. ) ;
#4509 = DIRECTION ( 'NONE',  ( 1.000000000000000000, 0.000000000000000000, 0.000000000000000000 ) ) ;
#4510 = TOROIDAL_SURFACE ( 'NONE', #11532, 11.50000000000000178, 0.5000000000000000000 ) ;
#4511 = ORIENTED_EDGE ( 'NONE', *, *, #5487, .T. ) ;
#4512 = CARTESIAN_POINT ( 'NONE',  ( 3.074695600507137083, -11.23985886659436773, -10.75417554975720869 ) ) ;
#4513 = CARTESIAN_POINT ( 'NONE',  ( 6.439472576468413756, -7.500000000000131450, -12.20506288372488690 ) ) ;
#4514 = ORIENTED_EDGE ( 'NONE', *, *, #9413, .F. ) ;
#4515 = DIRECTION ( 'NONE',  ( 0.000000000000000000, 0.000000000000000000, 1.000000000000000000 ) ) ;
#4516 = CARTESIAN_POINT ( 'NONE',  ( 1.342453679581834924, -7.902645620902353230, -12.51077660954474702 ) ) ;
#4517 = EDGE_CURVE ( 'NONE', #4248, #9121, #66, .T. ) ;
#4518 = DIRECTION ( 'NONE',  ( -1.000000000000000000, -0.000000000000000000, -0.000000000000000000 ) ) ;
#4519 = DIRECTION ( 'NONE',  ( 0.000000000000000000, 0.000000000000000000, 1.000000000000000000 ) ) ;
#4520 = ORIENTED_EDGE ( 'NONE', *, *, #1001, .T. ) ;
#4521 = EDGE_CURVE ( 'NONE', #4455, #7381, #13840, .T. ) ;
#4522 = AXIS2_PLACEMENT_3D ( 'NONE', #4617, #14358, #16084 ) ;
#4523 = CARTESIAN_POINT ( 'NONE',  ( 3.950837973638668288, 0.000000000000000000, 0.000000000000000000 ) ) ;
#4524 = CARTESIAN_POINT ( 'NONE',  ( 1.846138399168762101, -0.4167076046096411246, 12.43476674860266407 ) ) ;
#4525 = EDGE_CURVE ( 'NONE', #11172, #3195, #1550, .T. ) ;
#4526 = CARTESIAN_POINT ( 'NONE',  ( 16.56872352241294521, 0.004564908236400220913, 0.009382111268606271176 ) ) ;
#4527 = CARTESIAN_POINT ( 'NONE',  ( 1.254009781011257374, 12.44229282923036628, 7.789615163754328719 ) ) ;
#4528 = CARTESIAN_POINT ( 'NONE',  ( 2.747332970342022840, 16.12459247543629814, -2.705255688517677282 ) ) ;
#4529 = VERTEX_POINT ( 'NONE', #12777 ) ;
#4530 = CARTESIAN_POINT ( 'NONE',  ( 2.002547531651519996, 11.75462648437108015, -4.532360870844206246 ) ) ;
#4531 = CARTESIAN_POINT ( 'NONE',  ( 16.56753206892534891, 0.004253784598196178393, -0.008490833999798937798 ) ) ;
#4532 = TOROIDAL_SURFACE ( 'NONE', #6976, 3.499999999999994671, 0.5000000000000000000 ) ;
#4533 = VERTEX_POINT ( 'NONE', #18603 ) ;
#4534 = ORIENTED_EDGE ( 'NONE', *, *, #3756, .T. ) ;
#4535 = CARTESIAN_POINT ( 'NONE',  ( 0.8740764193766769052, -13.83508774436000088, 3.609949042658186169 ) ) ;
#4536 = EDGE_LOOP ( 'NONE', ( #8273, #13828, #6197, #7186 ) ) ;
#4537 = FACE_OUTER_BOUND ( 'NONE', #5213, .T. ) ;
#4538 = ORIENTED_EDGE ( 'NONE', *, *, #8316, .T. ) ;
#4539 = EDGE_CURVE ( 'NONE', #10086, #3893, #6235, .T. ) ;
#4540 = CARTESIAN_POINT ( 'NONE',  ( 0.4384471787762841966, -0.7363690479465361260, -13.84291427302852817 ) ) ;
#4541 = DIRECTION ( 'NONE',  ( -1.000000000000000000, -0.000000000000000000, -0.000000000000000000 ) ) ;
#4542 = CARTESIAN_POINT ( 'NONE',  ( 2.636624412716062960, -2.161493821598612808, -15.91454522070331912 ) ) ;
#4543 = CARTESIAN_POINT ( 'NONE',  ( 0.3132642857406535697, -13.21852905223341601, 3.740125687984681591 ) ) ;
#4544 = ADVANCED_FACE ( 'NONE', ( #4187 ), #10001, .T. ) ;
#4545 = CARTESIAN_POINT ( 'NONE',  ( -59.99999999999997158, -10.00000000000000888, 3.000000000000000000 ) ) ;
#4546 = CARTESIAN_POINT ( 'NONE',  ( 2.705023505549862151, -4.909285963183986468, -12.36217802824811152 ) ) ;
#4547 = CARTESIAN_POINT ( 'NONE',  ( 1.847340342630339860, 0.1245571717073309381, 12.44248139376886186 ) ) ;
#4548 = FACE_OUTER_BOUND ( 'NONE', #7524, .T. ) ;
#4549 = CARTESIAN_POINT ( 'NONE',  ( 0.3939822652208154752, 7.545099438012025317, 11.57634296752770453 ) ) ;
#4550 = LINE ( 'NONE', #16112, #12136 ) ;
#4551 = CARTESIAN_POINT ( 'NONE',  ( 0.000000000000000000, 0.000000000000000000, -3.000000000000000000 ) ) ;
#4552 = CARTESIAN_POINT ( 'NONE',  ( 1.977228804422059394, -15.33060379559095310, 1.488378900182341091 ) ) ;
#4553 = ORIENTED_EDGE ( 'NONE', *, *, #9404, .T. ) ;
#4554 = ORIENTED_EDGE ( 'NONE', *, *, #3216, .F. ) ;
#4555 = EDGE_LOOP ( 'NONE', ( #5703, #8496, #14934, #1218 ) ) ;
#4556 = ORIENTED_EDGE ( 'NONE', *, *, #18749, .F. ) ;
#4557 =( BOUNDED_SURFACE ( )  B_SPLINE_SURFACE ( 3, 1, ( 
 ( #16590, #17832 ),
 ( #13518, #6369 ),
 ( #12097, #10666 ),
 ( #13716, #2067 ) ),
 .UNSPECIFIED., .F., .F., .T. ) 
 B_SPLINE_SURFACE_WITH_KNOTS ( ( 4, 4 ),
 ( 2, 2 ),
 ( 0.000000000000000000, 1.000000000000000000 ),
 ( 0.000000000000000000, 1.000000000000000000 ),
 .UNSPECIFIED. ) 
 GEOMETRIC_REPRESENTATION_ITEM ( )  RATIONAL_B_SPLINE_SURFACE ( (
 ( 1.000000000000000000, 1.000000000000000000),
 ( 0.9933953342250436691, 0.8357391271907733676),
 ( 0.9933953342250436691, 0.8357391271907733676),
 ( 1.000000000000000000, 1.000000000000000000) ) ) 
 REPRESENTATION_ITEM ( '' )  SURFACE ( )  );
#4558 = EDGE_CURVE ( 'NONE', #10485, #15469, #16361, .T. ) ;
#4559 = CARTESIAN_POINT ( 'NONE',  ( 0.3150686449036074199, 0.1533607327085746430, 13.73846184595213771 ) ) ;
#4560 = FACE_OUTER_BOUND ( 'NONE', #10869, .T. ) ;
#4561 = DIRECTION ( 'NONE',  ( -1.000000000000000000, -5.782411586589358625E-16, 0.000000000000000000 ) ) ;
#4562 = ORIENTED_EDGE ( 'NONE', *, *, #14197, .T. ) ;
#4563 = DIRECTION ( 'NONE',  ( 0.000000000000000000, 1.000000000000000000, 0.000000000000000000 ) ) ;
#4564 = DIRECTION ( 'NONE',  ( 0.000000000000000000, 0.000000000000000000, 1.000000000000000000 ) ) ;
#4565 = CARTESIAN_POINT ( 'NONE',  ( 8.438534575730034959, -6.598402093327866424, -1.899950616255257740 ) ) ;
#4566 = CARTESIAN_POINT ( 'NONE',  ( 2.636624412714237309, 15.91454522070173638, -2.161493821596664144 ) ) ;
#4567 = CARTESIAN_POINT ( 'NONE',  ( 1.499999999999999112, 4.769696007084728073, -3.000000000000000000 ) ) ;
#4568 = CIRCLE ( 'NONE', #13723, 12.50000000000000355 ) ;
#4569 =( GEOMETRIC_REPRESENTATION_CONTEXT ( 3 ) GLOBAL_UNCERTAINTY_ASSIGNED_CONTEXT ( ( #9768 ) ) GLOBAL_UNIT_ASSIGNED_CONTEXT ( ( #11310, #5280, #1066 ) ) REPRESENTATION_CONTEXT ( 'NONE', 'WORKASPACE' ) );
#4570 = DIRECTION ( 'NONE',  ( 0.000000000000000000, 0.000000000000000000, -1.000000000000000000 ) ) ;
#4571 = CARTESIAN_POINT ( 'NONE',  ( 1.861628059977343597, -9.751736252960316875, -7.751680370225499495 ) ) ;
#4572 = CARTESIAN_POINT ( 'NONE',  ( 0.3137051932979792457, -10.83767969834796929, -8.442169467526971616 ) ) ;
#4573 = FACE_OUTER_BOUND ( 'NONE', #3370, .T. ) ;
#4574 = VECTOR ( 'NONE', #18016, 1000.000000000000114 ) ;
#4575 = ORIENTED_EDGE ( 'NONE', *, *, #7391, .T. ) ;
#4576 = VERTEX_POINT ( 'NONE', #17663 ) ;
#4577 = ORIENTED_EDGE ( 'NONE', *, *, #12513, .T. ) ;
#4578 = ORIENTED_EDGE ( 'NONE', *, *, #7039, .F. ) ;
#4579 = FACE_OUTER_BOUND ( 'NONE', #11931, .T. ) ;
#4580 = EDGE_CURVE ( 'NONE', #15061, #14742, #3345, .T. ) ;
#4581 = ORIENTED_EDGE ( 'NONE', *, *, #4472, .F. ) ;
#4582 = EDGE_CURVE ( 'NONE', #9014, #7450, #1971, .T. ) ;
#4583 = CARTESIAN_POINT ( 'NONE',  ( 1.918921323896324971, -6.832782632379298171, -10.48468902844559913 ) ) ;
#4584 = CARTESIAN_POINT ( 'NONE',  ( -55.93192566395838128, 9.999999999999973355, 3.000000000000000000 ) ) ;
#4585 = DIRECTION ( 'NONE',  ( 0.000000000000000000, 0.000000000000000000, -1.000000000000000000 ) ) ;
#4586 = CARTESIAN_POINT ( 'NONE',  ( 3.950837973638668288, 14.41405733518061538, -1.958075594453841273 ) ) ;
#4587 = VERTEX_POINT ( 'NONE', #453 ) ;
#4588 = CARTESIAN_POINT ( 'NONE',  ( -2.863953186090931524, 7.500000000000000888, -15.84864299207352012 ) ) ;
#4589 = DIRECTION ( 'NONE',  ( 0.8629742774544859607, -0.5052478564545405115, -0.000000000000000000 ) ) ;
#4590 = DIRECTION ( 'NONE',  ( 1.000000000000000000, 0.000000000000000000, 0.000000000000000000 ) ) ;
#4591 = CARTESIAN_POINT ( 'NONE',  ( 0.4754618798421162973, 12.98792082933651493, -5.007009103465114741 ) ) ;
#4592 = CARTESIAN_POINT ( 'NONE',  ( 1.342453679581834924, 14.76648944001039254, 0.9602753779831241232 ) ) ;
#4593 = CARTESIAN_POINT ( 'NONE',  ( 1.846138399168762101, 6.971848976711159551, -10.30487220521562541 ) ) ;
#4594 =( BOUNDED_SURFACE ( )  B_SPLINE_SURFACE ( 3, 1, ( 
 ( #7301, #8907 ),
 ( #10443, #14735 ),
 ( #13020, #1645 ),
 ( #17811, #14453 ) ),
 .UNSPECIFIED., .F., .F., .T. ) 
 B_SPLINE_SURFACE_WITH_KNOTS ( ( 4, 4 ),
 ( 2, 2 ),
 ( 0.000000000000000000, 1.000000000000000000 ),
 ( 0.000000000000000000, 1.000000000000000000 ),
 .UNSPECIFIED. ) 
 GEOMETRIC_REPRESENTATION_ITEM ( )  RATIONAL_B_SPLINE_SURFACE ( (
 ( 1.000000000000000000, 1.000000000000000000),
 ( 0.9933953342250438912, 0.8357391271907739227),
 ( 0.9933953342250438912, 0.8357391271907739227),
 ( 1.000000000000000000, 1.000000000000000000) ) ) 
 REPRESENTATION_ITEM ( '' )  SURFACE ( )  );
#4595 = CARTESIAN_POINT ( 'NONE',  ( 16.56753206892534891, 0.001421777558676785977, 0.009389754735541558373 ) ) ;
#4596 = ORIENTED_EDGE ( 'NONE', *, *, #801, .T. ) ;
#4597 = CARTESIAN_POINT ( 'NONE',  ( 2.636624412714134280, 2.862162146984768896, 15.80357026013147426 ) ) ;
#4599 = ORIENTED_EDGE ( 'NONE', *, *, #9977, .F. ) ;
#4598 = CYLINDRICAL_SURFACE ( 'NONE', #9372, 5.000000000000000000 ) ;
#4600 = CARTESIAN_POINT ( 'NONE',  ( 0.3151930723728414985, 8.137566970826528134, -11.07033375389122831 ) ) ;
#4601 = DIRECTION ( 'NONE',  ( 0.7635533937278216055, -0.3620487483322484823, -0.5347026451755951815 ) ) ;
#4602 = VERTEX_POINT ( 'NONE', #17952 ) ;
#4603 = CARTESIAN_POINT ( 'NONE',  ( 3.950837973638676281, 6.316429227969464932, 13.10350451991842569 ) ) ;
#4604 = UNCERTAINTY_MEASURE_WITH_UNIT (LENGTH_MEASURE( 1.000000000000000082E-05 ), #12759, 'distance_accuracy_value', 'NONE');
#4605 = CARTESIAN_POINT ( 'NONE',  ( 5.075684663107828065, -4.834325206103392780, -12.00000000445688464 ) ) ;
#4606 = ORIENTED_EDGE ( 'NONE', *, *, #3044, .F. ) ;
#4607 = PLANE ( 'NONE',  #18519 ) ;
#4608 = CARTESIAN_POINT ( 'NONE',  ( 0.3939822652208120890, -10.75310269629515325, -8.678192463540291612 ) ) ;
#4609 = EDGE_CURVE ( 'NONE', #18257, #18612, #5594, .T. ) ;
#4610 = CARTESIAN_POINT ( 'NONE',  ( 2.002547531651519996, 3.242439124566821818, -12.17374746633574745 ) ) ;
#4611 = CARTESIAN_POINT ( 'NONE',  ( 1.846138399168762101, -11.95493567637852905, 3.446241763652952539 ) ) ;
#4612 = VECTOR ( 'NONE', #7351, 1000.000000000000000 ) ;
#4613 = ORIENTED_EDGE ( 'NONE', *, *, #4521, .F. ) ;
#4614 = EDGE_CURVE ( 'NONE', #17792, #996, #7535, .T. ) ;
#4615 = SURFACE_STYLE_USAGE ( .BOTH. , #218 ) ;
#4616 = CARTESIAN_POINT ( 'NONE',  ( 0.4754618798421162973, 13.45049478164064638, -3.583352865732528425 ) ) ;
#4617 = CARTESIAN_POINT ( 'NONE',  ( 0.000000000000000000, 0.000000000000000000, -6.000000000000000000 ) ) ;
#4618 = CARTESIAN_POINT ( 'NONE',  ( 1.845756295923353330, 0.4783934145702027352, 12.43231724724607190 ) ) ;
#4619 = CARTESIAN_POINT ( 'NONE',  ( 2.002547531651519996, 0.6781519942173496185, -12.57989064830758785 ) ) ;
#4620 = CARTESIAN_POINT ( 'NONE',  ( 2.353870697619111940, -6.980654702310762794, -10.90705766126227871 ) ) ;
#4621 = ORIENTED_EDGE ( 'NONE', *, *, #1423, .F. ) ;
#4622 = CARTESIAN_POINT ( 'NONE',  ( 0.3148213771069373057, -8.260246460850796169, 10.97836617636221845 ) ) ;
#4623 = CARTESIAN_POINT ( 'NONE',  ( 0.3095370825347224519, -10.84046130709064570, 8.444334731363969837 ) ) ;
#4624 = VERTEX_POINT ( 'NONE', #13248 ) ;
#4625 = ORIENTED_EDGE ( 'NONE', *, *, #16628, .T. ) ;
#4627 = CARTESIAN_POINT ( 'NONE',  ( 3.686287386450715076E-15, -27.00000000000000000, 25.01316734529526187 ) ) ;
#4626 = AXIS2_PLACEMENT_3D ( 'NONE', #13967, #1244, #16931 ) ;
#4628 = ORIENTED_EDGE ( 'NONE', *, *, #8885, .T. ) ;
#4629 = CARTESIAN_POINT ( 'NONE',  ( 0.3720661004400037664, 4.951033743989821545, -12.89739157014187221 ) ) ;
#4630 = EDGE_CURVE ( 'NONE', #3711, #6002, #10295, .T. ) ;
#4631 = B_SPLINE_CURVE_WITH_KNOTS ( 'NONE', 3,
 ( #6473, #18037, #15526, #2170, #16601, #12298 ),
 .UNSPECIFIED., .F., .F.,
 ( 4, 2, 4 ),
 ( 4.005364051932256883E-17, 0.0002014099069817290285, 0.0004028198139634179956 ),
 .UNSPECIFIED. ) ;
#4632 = ORIENTED_EDGE ( 'NONE', *, *, #13975, .T. ) ;
#4633 = CARTESIAN_POINT ( 'NONE',  ( 3.950837973638675393, 6.888253895133479965, -12.81214529934967672 ) ) ;
#4634 = EDGE_CURVE ( 'NONE', #8377, #12041, #2259, .T. ) ;
#4635 = EDGE_CURVE ( 'NONE', #10713, #859, #12618, .T. ) ;
#4636 = CARTESIAN_POINT ( 'NONE',  ( 0.3151930723728451622, -13.73922999529477451, -0.07645105377001075453 ) ) ;
#4637 = FACE_OUTER_BOUND ( 'NONE', #1881, .T. ) ;
#4638 = CARTESIAN_POINT ( 'NONE',  ( 0.3150686449036049219, 4.391272911157320991, 13.01866258978838609 ) ) ;
#4639 = DIRECTION ( 'NONE',  ( 0.000000000000000000, 0.000000000000000000, 1.000000000000000000 ) ) ;
#4640 = CARTESIAN_POINT ( 'NONE',  ( 0.4862570985993235340, -0.7479633556563419772, 13.89016912371017121 ) ) ;
#4641 = CARTESIAN_POINT ( 'NONE',  ( 3.950837973638676281, 12.81214529934975310, 6.888253895133341409 ) ) ;
#4642 = DIRECTION ( 'NONE',  ( 0.000000000000000000, 0.000000000000000000, 1.000000000000000000 ) ) ;
#4643 = CARTESIAN_POINT ( 'NONE',  ( -199.9999999999999716, -5.000000000000024869, 6.000000000000000000 ) ) ;
#4644 = EDGE_CURVE ( 'NONE', #14303, #15038, #13554, .T. ) ;
#4645 = CARTESIAN_POINT ( 'NONE',  ( 0.4862570985993235340, 13.44146924561385958, -3.580942890621532371 ) ) ;
#4646 = VECTOR ( 'NONE', #2672, 1000.000000000000000 ) ;
#4647 = CARTESIAN_POINT ( 'NONE',  ( 16.56872352241294521, -0.007512283835805501873, -0.007240717549633963156 ) ) ;
#4648 = ORIENTED_EDGE ( 'NONE', *, *, #2382, .F. ) ;
#4649 = VERTEX_POINT ( 'NONE', #10587 ) ;
#4650 = ORIENTED_EDGE ( 'NONE', *, *, #18545, .T. ) ;
#4651 = ORIENTED_EDGE ( 'NONE', *, *, #490, .F. ) ;
#4652 = CARTESIAN_POINT ( 'NONE',  ( 1.845755665166724402, -9.776700214453573068, -7.694641135842929636 ) ) ;
#4653 = B_SPLINE_CURVE_WITH_KNOTS ( 'NONE', 3,
 ( #15211, #12516, #8320, #1037 ),
 .UNSPECIFIED., .F., .F.,
 ( 4, 4 ),
 ( 1.226634733346699349E-18, 0.003005512676784830983 ),
 .UNSPECIFIED. ) ;
#4654 = CARTESIAN_POINT ( 'NONE',  ( 16.56753206892534891, -0.009389754735541561842, 0.001421777558676752366 ) ) ;
#4655 = CARTESIAN_POINT ( 'NONE',  ( 3.664313757352974488, -12.97355833021536498, -5.926151963190507743 ) ) ;
#4656 = ORIENTED_EDGE ( 'NONE', *, *, #14925, .F. ) ;
#4657 = CARTESIAN_POINT ( 'NONE',  ( 20.00000000000000000, 2.499999999999998668, -17.00000000000000000 ) ) ;
#4658 = DIRECTION ( 'NONE',  ( 1.000000000000000000, 0.000000000000000000, 0.000000000000000000 ) ) ;
#4659 = DIRECTION ( 'NONE',  ( 1.000000000000000000, 0.000000000000000000, 0.000000000000000000 ) ) ;
#4660 = CARTESIAN_POINT ( 'NONE',  ( 0.4754618798421162973, -5.007009103465161814, -12.98792082933649539 ) ) ;
#4661 = CARTESIAN_POINT ( 'NONE',  ( 16.56872352241294521, -0.001821578298044716857, -0.01027347319884440967 ) ) ;
#4662 = AXIS2_PLACEMENT_3D ( 'NONE', #10167, #1189, #5567 ) ;
#4663 = EDGE_CURVE ( 'NONE', #13528, #5954, #12918, .T. ) ;
#4664 = CARTESIAN_POINT ( 'NONE',  ( 1.959283090834840646, -4.509128209890892691, -11.71721539537259282 ) ) ;
#4665 = CARTESIAN_POINT ( 'NONE',  ( 1.977228804421386821, 10.21522664410325021, 11.52787183731143017 ) ) ;
#4666 = B_SPLINE_CURVE_WITH_KNOTS ( 'NONE', 3,
 ( #17173, #4085, #12779, #11731, #1507, #3010 ),
 .UNSPECIFIED., .F., .F.,
 ( 4, 2, 4 ),
 ( 1.939479807224432123E-18, 0.001657017934710795738, 0.003314035869421589307 ),
 .UNSPECIFIED. ) ;
#4667 = CARTESIAN_POINT ( 'NONE',  ( 0.3145729642390400205, -11.29233589755986600, -7.825496023201434781 ) ) ;
#4668 = CARTESIAN_POINT ( 'NONE',  ( 0.3151930723728413319, 4.318364831037771800, -13.04315954105010533 ) ) ;
#4669 = CONICAL_SURFACE ( 'NONE', #7457, 2.055000000000000160, 0.7853981633974482790 ) ;
#4670 = EDGE_CURVE ( 'NONE', #18124, #4997, #12934, .T. ) ;
#4671 = ORIENTED_EDGE ( 'NONE', *, *, #1912, .T. ) ;
#4672 =( BOUNDED_SURFACE ( )  B_SPLINE_SURFACE ( 3, 1, ( 
 ( #5947, #1755 ),
 ( #7600, #17722 ),
 ( #13311, #11790 ),
 ( #7786, #9204 ) ),
 .UNSPECIFIED., .F., .F., .T. ) 
 B_SPLINE_SURFACE_WITH_KNOTS ( ( 4, 4 ),
 ( 2, 2 ),
 ( 0.000000000000000000, 1.000000000000000000 ),
 ( 0.000000000000000000, 1.000000000000000000 ),
 .UNSPECIFIED. ) 
 GEOMETRIC_REPRESENTATION_ITEM ( )  RATIONAL_B_SPLINE_SURFACE ( (
 ( 1.000000000000000000, 1.000000000000000000),
 ( 0.7792777138730158093, 0.9689936506012928330),
 ( 0.7792777138730158093, 0.9689936506012928330),
 ( 1.000000000000000000, 1.000000000000000000) ) ) 
 REPRESENTATION_ITEM ( '' )  SURFACE ( )  );
#4673 = ORIENTED_EDGE ( 'NONE', *, *, #6444, .F. ) ;
#4674 = EDGE_LOOP ( 'NONE', ( #6178, #16124, #36 ) ) ;
#4675 = ORIENTED_EDGE ( 'NONE', *, *, #12320, .T. ) ;
#4676 = DIRECTION ( 'NONE',  ( 0.000000000000000000, 0.000000000000000000, 1.000000000000000000 ) ) ;
#4677 = CARTESIAN_POINT ( 'NONE',  ( -199.9999999999999716, -25.00000000000003197, 3.000000000000000000 ) ) ;
#4678 = CARTESIAN_POINT ( 'NONE',  ( 1.846138399168762989, 11.69739621335922308, 4.238866729160444713 ) ) ;
#4679 = DIRECTION ( 'NONE',  ( -1.000000000000000000, 0.000000000000000000, 0.000000000000000000 ) ) ;
#4680 = ORIENTED_EDGE ( 'NONE', *, *, #13170, .T. ) ;
#4681 = CARTESIAN_POINT ( 'NONE',  ( 3.377929128793385249, 13.64476897106782971, 3.070552481924919253 ) ) ;
#4682 = CIRCLE ( 'NONE', #15046, 5.000000000000000000 ) ;
#4683 = CARTESIAN_POINT ( 'NONE',  ( 0.3145734862173258373, 12.96846406299306587, 4.535879238194977070 ) ) ;
#4684 = DIRECTION ( 'NONE',  ( 0.000000000000000000, 0.000000000000000000, 1.000000000000000000 ) ) ;
#4685 = DIRECTION ( 'NONE',  ( 0.000000000000000000, 0.000000000000000000, -1.000000000000000000 ) ) ;
#4686 = CARTESIAN_POINT ( 'NONE',  ( -194.9999999999999716, -15.00000000000003020, 6.000000000000005329 ) ) ;
#4687 = DIRECTION ( 'NONE',  ( -0.7635533937278216055, 0.02138673900301891681, 0.6453904417649388714 ) ) ;
#4688 = EDGE_CURVE ( 'NONE', #2296, #14986, #4708, .T. ) ;
#4689 = CARTESIAN_POINT ( 'NONE',  ( 3.512766787570699822, -13.55823433651950616, -6.535475144497160827 ) ) ;
#4690 = EDGE_CURVE ( 'NONE', #6415, #10542, #7147, .T. ) ;
#4691 = EDGE_CURVE ( 'NONE', #13997, #3393, #12293, .T. ) ;
#4692 = ORIENTED_EDGE ( 'NONE', *, *, #4826, .T. ) ;
#4693 = DIRECTION ( 'NONE',  ( 0.4246593920385850485, 0.1376957914266804250, -0.8948208031649687033 ) ) ;
#4695 = ORIENTED_EDGE ( 'NONE', *, *, #11637, .F. ) ;
#4694 = CARTESIAN_POINT ( 'NONE',  ( 3.950837973638677170, 10.51028938476232355, -10.05648675950114956 ) ) ;
#4696 = CARTESIAN_POINT ( 'NONE',  ( 0.4862570985993252548, 12.97920246947879441, 5.003653737315533867 ) ) ;
#4697 = CIRCLE ( 'NONE', #12020, 16.06066017081991149 ) ;
#4698 = AXIS2_PLACEMENT_3D ( 'NONE', #3197, #17551, #1499 ) ;
#4699 = CARTESIAN_POINT ( 'NONE',  ( 0.4385251269669976359, -4.978066129061780032, 12.93791070501032436 ) ) ;
#4700 = ORIENTED_EDGE ( 'NONE', *, *, #12074, .F. ) ;
#4701 = CARTESIAN_POINT ( 'NONE',  ( 0.3939822652208129217, -12.90851734139303453, -4.930560016699199188 ) ) ;
#4702 = CARTESIAN_POINT ( 'NONE',  ( 0.000000000000000000, 0.000000000000000000, -13.42403576283810906 ) ) ;
#4703 = ORIENTED_EDGE ( 'NONE', *, *, #4417, .F. ) ;
#4704 = DIRECTION ( 'NONE',  ( -0.7561779333270775005, 0.3559159372837393809, -0.5491072561318300904 ) ) ;
#4705 = CARTESIAN_POINT ( 'NONE',  ( 16.56872352241294521, 0.007240717549633990044, -0.007512283835805476720 ) ) ;
#4706 = DIRECTION ( 'NONE',  ( 1.049727191138619928E-16, 0.5150380749100523792, -0.8571673007021134438 ) ) ;
#4707 = CARTESIAN_POINT ( 'NONE',  ( 16.58200780006414732, 0.002844973367391573534, -0.01080144354108867819 ) ) ;
#4708 = CIRCLE ( 'NONE', #15382, 5.000000000000000000 ) ;
#4709 = VERTEX_POINT ( 'NONE', #1891 ) ;
#4710 = PRODUCT_DEFINITION_FORMATION_WITH_SPECIFIED_SOURCE ( 'ANY', '', #1414, .NOT_KNOWN. ) ;
#4711 = EDGE_CURVE ( 'NONE', #11930, #7450, #14880, .T. ) ;
#4712 = CARTESIAN_POINT ( 'NONE',  ( 2.747332970342022840, -14.49942876448597673, 7.555624153089596895 ) ) ;
#4713 = CARTESIAN_POINT ( 'NONE',  ( 12.00000000000000178, 0.000000000000000000, 10.49999999999999822 ) ) ;
#4714 = EDGE_CURVE ( 'NONE', #767, #3595, #18877, .T. ) ;
#4715 = CARTESIAN_POINT ( 'NONE',  ( 16.56753206892534891, 0.004368917149004243779, -0.008432171035096398468 ) ) ;
#4716 = CARTESIAN_POINT ( 'NONE',  ( 1.977228804421389485, 13.27756617201186096, 7.806978995470745808 ) ) ;
#4717 = CARTESIAN_POINT ( 'NONE',  ( 2.636624412715137034, -11.60464335004055947, 11.10302021257951743 ) ) ;
#4718 = EDGE_CURVE ( 'NONE', #5038, #9139, #16858, .T. ) ;
#4719 = ORIENTED_EDGE ( 'NONE', *, *, #5927, .F. ) ;
#4720 = CARTESIAN_POINT ( 'NONE',  ( 2.705023505549867924, 12.36217802824812573, -4.909285963183943835 ) ) ;
#4721 = CARTESIAN_POINT ( 'NONE',  ( 2.705023505549867036, 12.88681800078732387, 3.294610156755938934 ) ) ;
#4722 = ORIENTED_EDGE ( 'NONE', *, *, #6828, .T. ) ;
#4723 = VERTEX_POINT ( 'NONE', #3502 ) ;
#4724 = CARTESIAN_POINT ( 'NONE',  ( -66.35602477868049220, -10.00000000000000888, 11.00000000000000000 ) ) ;
#4725 = EDGE_LOOP ( 'NONE', ( #2509, #11743, #18683, #495 ) ) ;
#4726 = CARTESIAN_POINT ( 'NONE',  ( 16.56872352241294521, -0.01027347319884440620, 0.001821578298044753286 ) ) ;
#4727 = ADVANCED_FACE ( 'NONE', ( #4944 ), #6474, .T. ) ;
#4728 = ORIENTED_EDGE ( 'NONE', *, *, #14023, .F. ) ;
#4729 = FILL_AREA_STYLE ('',( #17632 ) ) ;
#4730 = CARTESIAN_POINT ( 'NONE',  ( 3.512766787570694493, 2.025881399556607843, -14.91422000116826041 ) ) ;
#4731 = CARTESIAN_POINT ( 'NONE',  ( 0.4862570985993235340, -13.44146924561383827, 3.580942890621619412 ) ) ;
#4732 = CARTESIAN_POINT ( 'NONE',  ( 0.3137051932979792457, 12.91601973349270871, 4.679953077377533965 ) ) ;
#4733 = CARTESIAN_POINT ( 'NONE',  ( 0.000000000000000000, -0.8660254037844384856, -1.500000000000000000 ) ) ;
#4734 = VECTOR ( 'NONE', #13350, 1000.000000000000000 ) ;
#4735 = DIRECTION ( 'NONE',  ( 0.000000000000000000, 0.000000000000000000, 1.000000000000000000 ) ) ;
#4736 = DIRECTION ( 'NONE',  ( -1.000000000000000000, 0.000000000000000000, 0.000000000000000000 ) ) ;
#4737 = AXIS2_PLACEMENT_3D ( 'NONE', #1920, #10710, #7371 ) ;
#4738 = CARTESIAN_POINT ( 'NONE',  ( 0.3308579732647042304, 7.595989242675130093, 11.46737410776356469 ) ) ;
#4739 = CONICAL_SURFACE ( 'NONE', #10538, 14.54644660717763927, 0.8559913436420816257 ) ;
#4740 = CARTESIAN_POINT ( 'NONE',  ( 0.3137051932979757485, -4.679953077377398074, -12.91601973349275134 ) ) ;
#4741 = EDGE_CURVE ( 'NONE', #14233, #2734, #10121, .T. ) ;
#4742 = CARTESIAN_POINT ( 'NONE',  ( 16.56753206892534891, -0.009369540855502119653, -0.001549402974393242162 ) ) ;
#4743 = CARTESIAN_POINT ( 'NONE',  ( 1.254009781011620417, -14.64464726212587919, 1.011465182608038305 ) ) ;
#4744 = ORIENTED_EDGE ( 'NONE', *, *, #13858, .T. ) ;
#4745 = VERTEX_POINT ( 'NONE', #15658 ) ;
#4746 = ORIENTED_EDGE ( 'NONE', *, *, #9977, .T. ) ;
#4747 = VERTEX_POINT ( 'NONE', #4008 ) ;
#4748 = CARTESIAN_POINT ( 'NONE',  ( 0.3151928478948580192, 0.0001388664989280257334, 13.73922860964089665 ) ) ;
#4749 = VECTOR ( 'NONE', #18648, 1000.000000000000000 ) ;
#4750 = CARTESIAN_POINT ( 'NONE',  ( -1.500000000000000000, -2.869946927167511679E-16, 5.000000000000000000 ) ) ;
#4751 = VECTOR ( 'NONE', #173, 1000.000000000000000 ) ;
#4752 = CARTESIAN_POINT ( 'NONE',  ( 1.846955891736115740, -12.44001089941741967, 0.2634721419534765685 ) ) ;
#4753 = CARTESIAN_POINT ( 'NONE',  ( -25.00000000000000000, -7.500000000000000888, -16.99999999999999645 ) ) ;
#4754 = CARTESIAN_POINT ( 'NONE',  ( 18.75000000000000000, 0.000000000000000000, 0.000000000000000000 ) ) ;
#4755 = EDGE_CURVE ( 'NONE', #18593, #859, #7976, .T. ) ;
#4756 = DIRECTION ( 'NONE',  ( -1.000000000000000000, -0.000000000000000000, -0.000000000000000000 ) ) ;
#4757 = CARTESIAN_POINT ( 'NONE',  ( 16.58200780006414732, 0.006043560077721704844, 0.009393638146079782980 ) ) ;
#4758 = DIRECTION ( 'NONE',  ( -0.000000000000000000, 1.000000000000000000, -0.000000000000000000 ) ) ;
#4759 = CARTESIAN_POINT ( 'NONE',  ( 1.847034903785825799, 0.2299360331935915713, -12.44051878787772480 ) ) ;
#4760 = CARTESIAN_POINT ( 'NONE',  ( 0.4862570985993252548, -3.580942890621766406, 13.44146924561379741 ) ) ;
#4761 = CARTESIAN_POINT ( 'NONE',  ( 2.369999999999999662, 4.749999999999999112, 0.000000000000000000 ) ) ;
#4762 = CARTESIAN_POINT ( 'NONE',  ( -66.35602477868047799, 9.999999999999973355, 5.999999999999999112 ) ) ;
#4763 = ORIENTED_EDGE ( 'NONE', *, *, #12688, .T. ) ;
#4764 = AXIS2_PLACEMENT_3D ( 'NONE', #17152, #1194, #18673 ) ;
#4765 = ORIENTED_EDGE ( 'NONE', *, *, #2853, .F. ) ;
#4766 = VERTEX_POINT ( 'NONE', #7168 ) ;
#4767 = ORIENTED_EDGE ( 'NONE', *, *, #7354, .F. ) ;
#4768 = CARTESIAN_POINT ( 'NONE',  ( 1.560000000000000053, 0.000000000000000000, 0.000000000000000000 ) ) ;
#4769 = EDGE_CURVE ( 'NONE', #846, #3169, #11560, .T. ) ;
#4770 = CARTESIAN_POINT ( 'NONE',  ( 16.56753206892534891, 0.004253784598196176658, -0.008490833999798941267 ) ) ;
#4771 = DIRECTION ( 'NONE',  ( 0.000000000000000000, 0.000000000000000000, -1.000000000000000000 ) ) ;
#4772 = CARTESIAN_POINT ( 'NONE',  ( 0.3720661004400040439, 4.951033743989640357, 12.89739157014194859 ) ) ;
#4773 = DIRECTION ( 'NONE',  ( -0.7635533937278214944, 0.3966532189476597581, 0.5095610256143870975 ) ) ;
#4774 = ORIENTED_EDGE ( 'NONE', *, *, #3647, .T. ) ;
#4775 = CARTESIAN_POINT ( 'NONE',  ( 2.002547531651519996, 12.17374746633578475, 3.242439124566693476 ) ) ;
#4776 = CARTESIAN_POINT ( 'NONE',  ( 0.3720661004400037664, -7.524064345033377954, -11.58636699658223179 ) ) ;
#4777 = AXIS2_PLACEMENT_3D ( 'NONE', #6838, #8006, #15436 ) ;
#4778 = DIRECTION ( 'NONE',  ( -1.000000000000000000, 0.000000000000000000, 0.000000000000000000 ) ) ;
#4779 = CARTESIAN_POINT ( 'NONE',  ( 2.747332970342022840, -2.705255688517959722, 16.12459247543625551 ) ) ;
#4780 =( GEOMETRIC_REPRESENTATION_CONTEXT ( 3 ) GLOBAL_UNCERTAINTY_ASSIGNED_CONTEXT ( ( #3080 ) ) GLOBAL_UNIT_ASSIGNED_CONTEXT ( ( #13302, #13017, #8903 ) ) REPRESENTATION_CONTEXT ( 'NONE', 'WORKASPACE' ) );
#4781 = CARTESIAN_POINT ( 'NONE',  ( 2.002547531651519996, 4.532360870844327039, 11.75462648437103752 ) ) ;
#4782 = ADVANCED_FACE ( 'NONE', ( #18621 ), #7775, .T. ) ;
#4783 = CARTESIAN_POINT ( 'NONE',  ( 0.4862570985993235340, 13.89016912371017476, -0.7479633556562934604 ) ) ;
#4784 =( BOUNDED_SURFACE ( )  B_SPLINE_SURFACE ( 3, 1, ( 
 ( #15797, #2690 ),
 ( #8537, #7106 ),
 ( #11506, #4243 ),
 ( #15980, #17421 ) ),
 .UNSPECIFIED., .F., .F., .F. ) 
 B_SPLINE_SURFACE_WITH_KNOTS ( ( 4, 4 ),
 ( 2, 2 ),
 ( 0.000000000000000000, 1.000000000000000000 ),
 ( 0.000000000000000000, 1.000000000000000000 ),
 .UNSPECIFIED. ) 
 GEOMETRIC_REPRESENTATION_ITEM ( )  RATIONAL_B_SPLINE_SURFACE ( (
 ( 1.000000000000000000, 1.000000000000000000),
 ( 0.7792777138730160313, 0.9689936506012927220),
 ( 0.7792777138730160313, 0.9689936506012927220),
 ( 1.000000000000000000, 1.000000000000000000) ) ) 
 REPRESENTATION_ITEM ( '' )  SURFACE ( )  );
#4785 = VERTEX_POINT ( 'NONE', #15945 ) ;
#4786 = CARTESIAN_POINT ( 'NONE',  ( 0.8740779401508858015, -11.05257166392043722, 9.070947476926702890 ) ) ;
#4788 = EDGE_LOOP ( 'NONE', ( #12454, #11557 ) ) ;
#4787 = CARTESIAN_POINT ( 'NONE',  ( 0.3095370825347224519, 10.84046130709058886, 8.444334731364044444 ) ) ;
#4789 = LINE ( 'NONE', #12247, #16996 ) ;
#4790 = AXIS2_PLACEMENT_3D ( 'NONE', #7401, #16183, #2876 ) ;
#4791 = CARTESIAN_POINT ( 'NONE',  ( 0.3095370825347224519, 7.700448427572037069, -11.38092634279620263 ) ) ;
#4792 =( GEOMETRIC_REPRESENTATION_CONTEXT ( 3 ) GLOBAL_UNCERTAINTY_ASSIGNED_CONTEXT ( ( #17636 ) ) GLOBAL_UNIT_ASSIGNED_CONTEXT ( ( #9937, #13963, #11205 ) ) REPRESENTATION_CONTEXT ( 'NONE', 'WORKASPACE' ) );
#4793 = B_SPLINE_CURVE_WITH_KNOTS ( 'NONE', 3,
 ( #3835, #18447, #14061, #15491 ),
 .UNSPECIFIED., .F., .F.,
 ( 4, 4 ),
 ( 6.158879127553505933E-17, 0.002004993803842649181 ),
 .UNSPECIFIED. ) ;
#4794 = AXIS2_PLACEMENT_3D ( 'NONE', #11229, #17043, #4037 ) ;
#4795 = ORIENTED_EDGE ( 'NONE', *, *, #7528, .F. ) ;
#4796 = DIRECTION ( 'NONE',  ( -2.891205793294679312E-16, 1.000000000000000000, 0.000000000000000000 ) ) ;
#4797 = PRODUCT_DEFINITION_SHAPE ( 'NONE', 'NONE',  #5434 ) ;
#4798 = CARTESIAN_POINT ( 'NONE',  ( -2.067729357296066883, -7.500000000000000888, -15.30380495029759480 ) ) ;
#4799 = EDGE_CURVE ( 'NONE', #12775, #4529, #5903, .T. ) ;
#4800 = VERTEX_POINT ( 'NONE', #8407 ) ;
#4801 = DIRECTION ( 'NONE',  ( 0.5547001962252284812, 0.8320502943378440541, 0.000000000000000000 ) ) ;
#4802 = ADVANCED_FACE ( 'NONE', ( #14414 ), #3317, .F. ) ;
#4803 = CARTESIAN_POINT ( 'NONE',  ( 0.3142014840576500267, 13.73311050063163918, 0.3830336514509360413 ) ) ;
#4804 = VECTOR ( 'NONE', #10036, 1000.000000000000114 ) ;
#4805 = CARTESIAN_POINT ( 'NONE',  ( 1.959212340397946450, 11.71715421693498449, 4.509090217468559203 ) ) ;
#4806 = CARTESIAN_POINT ( 'NONE',  ( 0.4385251269669978580, 3.577373010348713134, 13.39302348765809825 ) ) ;
#4807 = AXIS2_PLACEMENT_3D ( 'NONE', #14477, #14300, #11159 ) ;
#4808 = AXIS2_PLACEMENT_3D ( 'NONE', #7609, #12190, #7799 ) ;
#4809 = ORIENTED_EDGE ( 'NONE', *, *, #695, .T. ) ;
#4810 = CLOSED_SHELL ( 'NONE', ( #15173, #18029, #2164, #10355, #172, #2304 ) ) ;
#4811 = CARTESIAN_POINT ( 'NONE',  ( 16.57210152137263393, -0.005118120558002011225, -0.01361613799508959964 ) ) ;
#4812 = LINE ( 'NONE', #15468, #10950 ) ;
#4813 = CARTESIAN_POINT ( 'NONE',  ( 16.56782317627811096, 0.005492611183757310257, -0.008141063682853423578 ) ) ;
#4815 = ORIENTED_EDGE ( 'NONE', *, *, #1020, .F. ) ;
#4814 = CARTESIAN_POINT ( 'NONE',  ( 16.57778382496167424, 0.01482878558584569718, 0.001819584982831951199 ) ) ;
#4816 = CARTESIAN_POINT ( 'NONE',  ( 3.950837973638675393, -10.51028938476224894, 10.05648675950122595 ) ) ;
#4817 = VERTEX_POINT ( 'NONE', #2934 ) ;
#4818 = CARTESIAN_POINT ( 'NONE',  ( 0.3151926232592506816, -4.172630140040890723, 13.09050869763091107 ) ) ;
#4819 = CARTESIAN_POINT ( 'NONE',  ( 16.56872352241294521, 0.004564908236399969378, -0.009382111268607383134 ) ) ;
#4820 = EDGE_LOOP ( 'NONE', ( #5513, #14002, #18082, #4091 ) ) ;
#4821 = ORIENTED_EDGE ( 'NONE', *, *, #17337, .F. ) ;
#4822 = CARTESIAN_POINT ( 'NONE',  ( 0.3142011359265348691, 10.88514493056454135, -8.382042760265784764 ) ) ;
#4823 = ORIENTED_EDGE ( 'NONE', *, *, #12286, .T. ) ;
#4824 = CARTESIAN_POINT ( 'NONE',  ( 3.074695600507125981, -2.772091048739183439, -15.30693405987811673 ) ) ;
#4825 = VERTEX_POINT ( 'NONE', #14330 ) ;
#4826 = EDGE_CURVE ( 'NONE', #9203, #7454, #11654, .T. ) ;
#4827 = ADVANCED_FACE ( 'NONE', ( #17194 ), #13249, .T. ) ;
#4828 = EDGE_CURVE ( 'NONE', #18407, #7261, #12630, .T. ) ;
#4829 = FACE_OUTER_BOUND ( 'NONE', #686, .T. ) ;
#4830 = CARTESIAN_POINT ( 'NONE',  ( 0.3137051932979792457, -13.73004976592201842, -0.4596302728641207813 ) ) ;
#4831 = CARTESIAN_POINT ( 'NONE',  ( 1.846138399168762101, 9.815003036200520725, -7.646096044339786069 ) ) ;
#4832 = CARTESIAN_POINT ( 'NONE',  ( 0.3137051932979809665, 3.805684345189785933, 13.20008686438107581 ) ) ;
#4833 = VECTOR ( 'NONE', #7619, 1000.000000000000000 ) ;
#4834 = CARTESIAN_POINT ( 'NONE',  ( 0.3145734862173242274, -0.3064017202076312341, 13.73540602248381148 ) ) ;
#4835 = LINE ( 'NONE', #1334, #16033 ) ;
#4836 = CARTESIAN_POINT ( 'NONE',  ( 3.664313757352960721, 14.16986885736091750, 1.627055439596312159 ) ) ;
#4837 = CARTESIAN_POINT ( 'NONE',  ( 3.512766787570925864, 13.25664064834466593, -7.127386085302575225 ) ) ;
#4838 = ORIENTED_EDGE ( 'NONE', *, *, #2185, .F. ) ;
#4839 = CARTESIAN_POINT ( 'NONE',  ( 0.3145734862173244495, 7.825584895511528138, 11.29227530924448430 ) ) ;
#4840 = LINE ( 'NONE', #720, #11810 ) ;
#4841 = CARTESIAN_POINT ( 'NONE',  ( 1.846524061778021419, -11.71897913237546263, -4.180439405448447054 ) ) ;
#4842 = CARTESIAN_POINT ( 'NONE',  ( 0.3939875929385635023, -7.545068896001288827, 11.57636969881031241 ) ) ;
#4843 = ORIENTED_EDGE ( 'NONE', *, *, #13834, .F. ) ;
#4844 = ORIENTED_EDGE ( 'NONE', *, *, #4688, .F. ) ;
#4845 = ORIENTED_EDGE ( 'NONE', *, *, #10541, .F. ) ;
#4846 = ORIENTED_EDGE ( 'NONE', *, *, #3888, .F. ) ;
#4847 = CARTESIAN_POINT ( 'NONE',  ( 0.3148213771069321987, -7.888490156175138601, -11.24846294176320960 ) ) ;
#4848 = FACE_OUTER_BOUND ( 'NONE', #17818, .T. ) ;
#4849 = CARTESIAN_POINT ( 'NONE',  ( 0.3095370825347234511, -12.91933430393604532, -4.681152801286298626 ) ) ;
#4850 = LINE ( 'NONE', #7633, #18753 ) ;
#4851 = DIRECTION ( 'NONE',  ( 0.000000000000000000, 0.000000000000000000, 1.000000000000000000 ) ) ;
#4853 = ADVANCED_FACE ( 'NONE', ( #18712 ), #9188, .F. ) ;
#4852 = PRODUCT_DEFINITION_CONTEXT ( 'detailed design', #4115, 'design' ) ;
#4854 = CARTESIAN_POINT ( 'NONE',  ( 0.4862570985993235340, 0.7479633556564388996, -13.89016912371016765 ) ) ;
#4855 = CARTESIAN_POINT ( 'NONE',  ( 2.002547531651519996, 11.75462648437108015, -4.532360870844206246 ) ) ;
#4856 = CARTESIAN_POINT ( 'NONE',  ( 16.56822296793089322, -0.0007467251401297892322, -0.01011126603341077311 ) ) ;
#4857 = CARTESIAN_POINT ( 'NONE',  ( 16.57210152137263393, -0.01136813053532068768, -0.009075239946108325934 ) ) ;
#4858 = CARTESIAN_POINT ( 'NONE',  ( 16.56822296793089322, -0.01011126603341003585, -0.0007467251401289729364 ) ) ;
#4859 = CARTESIAN_POINT ( 'NONE',  ( 16.56753206892534891, -0.004368917149005391298, -0.008432171035096433162 ) ) ;
#4860 = FACE_OUTER_BOUND ( 'NONE', #3614, .T. ) ;
#4861 = ADVANCED_FACE ( 'NONE', ( #13174 ), #5904, .T. ) ;
#4862 = ORIENTED_EDGE ( 'NONE', *, *, #1916, .T. ) ;
#4863 = ORIENTED_EDGE ( 'NONE', *, *, #8438, .F. ) ;
#4864 = ORIENTED_EDGE ( 'NONE', *, *, #15449, .T. ) ;
#4865 = ORIENTED_EDGE ( 'NONE', *, *, #11732, .F. ) ;
#4866 = CARTESIAN_POINT ( 'NONE',  ( 1.846822687350015757, -7.075150813727044685, -10.23524390843947529 ) ) ;
#4867 = CARTESIAN_POINT ( 'NONE',  ( 16.56822296793089322, 0.002414375228568254022, -0.009847136207496285168 ) ) ;
#4868 = CARTESIAN_POINT ( 'NONE',  ( 2.320520222539028232, 15.43440824797023225, -3.126729907237324912 ) ) ;
#4869 = PRODUCT_RELATED_PRODUCT_CATEGORY ( 'part', '', ( #3577 ) ) ;
#4870 = CARTESIAN_POINT ( 'NONE',  ( 1.977436885025426694, 15.33079650480377154, 1.488549889121579817 ) ) ;
#4871 = CIRCLE ( 'NONE', #9737, 16.06066017081991149 ) ;
#4872 = EDGE_CURVE ( 'NONE', #13406, #8344, #2744, .T. ) ;
#4873 = CARTESIAN_POINT ( 'NONE',  ( 2.002547531651519996, -11.75462648437105173, 4.532360870844282630 ) ) ;
#4874 = ORIENTED_EDGE ( 'NONE', *, *, #3454, .T. ) ;
#4875 = CIRCLE ( 'NONE', #16472, 5.315148208181396328 ) ;
#4876 = CARTESIAN_POINT ( 'NONE',  ( 3.950837973638676281, 14.31366178983253512, 2.591948120961855118 ) ) ;
#4877 = DIRECTION ( 'NONE',  ( -0.000000000000000000, -0.000000000000000000, 1.000000000000000000 ) ) ;
#4878 = EDGE_CURVE ( 'NONE', #10634, #13856, #2009, .T. ) ;
#4879 = ADVANCED_FACE ( 'NONE', ( #14700 ), #764, .F. ) ;
#4880 = CARTESIAN_POINT ( 'NONE',  ( -3.648056509801823388, 7.499999999999999112, -16.29094785500086573 ) ) ;
#4881 = CARTESIAN_POINT ( 'NONE',  ( 1.846524061778018311, -10.27028962889602148, 7.023652644192237560 ) ) ;
#4882 =( GEOMETRIC_REPRESENTATION_CONTEXT ( 3 ) GLOBAL_UNCERTAINTY_ASSIGNED_CONTEXT ( ( #11314 ) ) GLOBAL_UNIT_ASSIGNED_CONTEXT ( ( #10749, #6361, #15236 ) ) REPRESENTATION_CONTEXT ( 'NONE', 'WORKASPACE' ) );
#4883 = CARTESIAN_POINT ( 'NONE',  ( 2.705023505549864371, 4.909285963184069956, 12.36217802824807421 ) ) ;
#4884 = CARTESIAN_POINT ( 'NONE',  ( 16.56872352241294521, -0.009207754980064163791, 0.004907101719995779661 ) ) ;
#4885 = CARTESIAN_POINT ( 'NONE',  ( 0.3142011359265314829, 12.94258167753018895, -4.608101617236642689 ) ) ;
#4886 = B_SPLINE_CURVE_WITH_KNOTS ( 'NONE', 3,
 ( #11952, #10520, #389, #13918, #6670, #8982 ),
 .UNSPECIFIED., .F., .F.,
 ( 4, 2, 4 ),
 ( 3.499941646806256644E-17, 0.0001825746017570582086, 0.0003651492035140814518 ),
 .UNSPECIFIED. ) ;
#4887 = ORIENTED_EDGE ( 'NONE', *, *, #408, .T. ) ;
#4888 = CARTESIAN_POINT ( 'NONE',  ( 0.4862570985993252548, 12.97920246947879441, 5.003653737315533867 ) ) ;
#4890 = EDGE_LOOP ( 'NONE', ( #1495, #927 ) ) ;
#4889 = CARTESIAN_POINT ( 'NONE',  ( 16.57778382496167424, 0.007244066302946777433, 0.01306626476309292149 ) ) ;
#4891 = LINE ( 'NONE', #1829, #18513 ) ;
#4892 = ADVANCED_FACE ( 'NONE', ( #13268 ), #8875, .T. ) ;
#4893 = CARTESIAN_POINT ( 'NONE',  ( 0.3137051932979775248, 10.83767969834815581, -8.442169467526731808 ) ) ;
#4894 = VERTEX_POINT ( 'NONE', #10612 ) ;
#4895 = CARTESIAN_POINT ( 'NONE',  ( 16.56753206892534891, 0.009369540855502530782, -0.001549402974394192573 ) ) ;
#4896 = CARTESIAN_POINT ( 'NONE',  ( 0.4158217634471226276, -7.500000000000000888, -14.24727159067851368 ) ) ;
#4897 = ORIENTED_EDGE ( 'NONE', *, *, #15609, .F. ) ;
#4898 = CARTESIAN_POINT ( 'NONE',  ( 1.560000000000000053, 0.8660254037844389297, -1.500000000000000000 ) ) ;
#4899 = CARTESIAN_POINT ( 'NONE',  ( 8.438534575730034959, -6.862570336891077538, 0.2320579683289888395 ) ) ;
#4900 = CARTESIAN_POINT ( 'NONE',  ( 0.3308579732646986238, -7.595989242675048381, -11.46737410776362509 ) ) ;
#4901 = DIRECTION ( 'NONE',  ( 0.000000000000000000, 0.000000000000000000, -1.000000000000000000 ) ) ;
#4902 = VERTEX_POINT ( 'NONE', #9072 ) ;
#4903 = LINE ( 'NONE', #3556, #8350 ) ;
#4904 = B_SPLINE_CURVE_WITH_KNOTS ( 'NONE', 3,
 ( #15505, #1064, #5189, #12819 ),
 .UNSPECIFIED., .F., .F.,
 ( 4, 4 ),
 ( 0.000000000000000000, 0.002004993803842713366 ),
 .UNSPECIFIED. ) ;
#4905 = CARTESIAN_POINT ( 'NONE',  ( 16.56822296793089322, 0.006547366384935510326, -0.007741272030791107074 ) ) ;
#4907 = EDGE_LOOP ( 'NONE', ( #2976, #5526, #8634, #1539 ) ) ;
#4906 = DIRECTION ( 'NONE',  ( 0.000000000000000000, 0.000000000000000000, 1.000000000000000000 ) ) ;
#4908 = CARTESIAN_POINT ( 'NONE',  ( 16.56782317627811096, -0.009814734722107087972, -0.0003415813796005906337 ) ) ;
#4909 = EDGE_CURVE ( 'NONE', #18033, #5504, #7459, .T. ) ;
#4910 = ORIENTED_EDGE ( 'NONE', *, *, #1863, .F. ) ;
#4911 = CARTESIAN_POINT ( 'NONE',  ( 1.254255976357675717, -14.64488542023465101, -1.011593778944541278 ) ) ;
#4912 = CARTESIAN_POINT ( 'NONE',  ( 2.636624412714237309, 7.605649742761960042, 14.14563173255213613 ) ) ;
#4913 = ORIENTED_EDGE ( 'NONE', *, *, #12538, .T. ) ;
#4914 = ORIENTED_EDGE ( 'NONE', *, *, #17637, .F. ) ;
#4915 = LINE ( 'NONE', #11888, #5141 ) ;
#4916 = VERTEX_POINT ( 'NONE', #16442 ) ;
#4917 = DIRECTION ( 'NONE',  ( 0.000000000000000000, 0.000000000000000000, 1.000000000000000000 ) ) ;
#4918 = EDGE_LOOP ( 'NONE', ( #4072, #4395, #2809 ) ) ;
#4919 = CARTESIAN_POINT ( 'NONE',  ( -25.00000000000000000, 2.499999999999998668, -12.00000000000000000 ) ) ;
#4920 = PRESENTATION_STYLE_ASSIGNMENT (( #15043 ) ) ;
#4921 = FACE_OUTER_BOUND ( 'NONE', #16434, .T. ) ;
#4922 = CARTESIAN_POINT ( 'NONE',  ( 1.846138399168762101, 11.69739621335927815, -4.238866729160283064 ) ) ;
#4923 = CARTESIAN_POINT ( 'NONE',  ( 2.002547531651520885, -4.532360870844412304, 11.75462648437100377 ) ) ;
#4924 = CARTESIAN_POINT ( 'NONE',  ( 0.3148213771069364175, -0.2297580318215671491, 13.73693585713734144 ) ) ;
#4925 = CARTESIAN_POINT ( 'NONE',  ( 16.56872352241294521, 0.009382111268607367521, 0.004564908236399998868 ) ) ;
#4926 = CARTESIAN_POINT ( 'NONE',  ( 1.846138399168762101, -10.30487220521565028, -6.971848976711123136 ) ) ;
#4927 = CARTESIAN_POINT ( 'NONE',  ( 0.3137051932979792457, 0.4596302728641686874, -13.73004976592201487 ) ) ;
#4928 = CARTESIAN_POINT ( 'NONE',  ( 0.3145729642390364678, 8.321438378985256179, 10.93201268464375353 ) ) ;
#4929 = CARTESIAN_POINT ( 'NONE',  ( -27.50000000000000711, -12.50000000000000178, 3.000000000000000000 ) ) ;
#4930 = ADVANCED_FACE ( 'NONE', ( #1611 ), #16516, .F. ) ;
#4931 = EDGE_CURVE ( 'NONE', #16009, #6505, #18439, .T. ) ;
#4932 = EDGE_CURVE ( 'NONE', #16968, #10713, #9111, .T. ) ;
#4933 = AXIS2_PLACEMENT_3D ( 'NONE', #13677, #13568, #493 ) ;
#4934 = CARTESIAN_POINT ( 'NONE',  ( 1.847168016377984889, -11.89018175117591980, -3.666915430942724097 ) ) ;
#4935 = VERTEX_POINT ( 'NONE', #9166 ) ;
#4936 = ORIENTED_EDGE ( 'NONE', *, *, #2348, .T. ) ;
#4937 = ORIENTED_EDGE ( 'NONE', *, *, #17064, .T. ) ;
#4938 = ORIENTED_EDGE ( 'NONE', *, *, #6158, .T. ) ;
#4939 = ORIENTED_EDGE ( 'NONE', *, *, #16581, .T. ) ;
#4940 = B_SPLINE_CURVE_WITH_KNOTS ( 'NONE', 3,
 ( #15688, #15788, #14080, #6818, #2774, #8531 ),
 .UNSPECIFIED., .F., .F.,
 ( 4, 2, 4 ),
 ( 3.522439207679730663E-17, 0.0001825746017570583171, 0.0003651492035140813976 ),
 .UNSPECIFIED. ) ;
#4941 = CARTESIAN_POINT ( 'NONE',  ( 1.918921323896324971, 0.6349083173281891979, -12.49850046818173688 ) ) ;
#4942 = EDGE_CURVE ( 'NONE', #18779, #4000, #5017, .T. ) ;
#4943 = CARTESIAN_POINT ( 'NONE',  ( 5.051325721637065058, -7.500000000000001776, -16.81741242948696069 ) ) ;
#4944 = FACE_OUTER_BOUND ( 'NONE', #14107, .T. ) ;
#4945 = ORIENTED_EDGE ( 'NONE', *, *, #10626, .T. ) ;
#4946 = CARTESIAN_POINT ( 'NONE',  ( 16.57210152137263393, -0.01361613799508957709, 0.005118120558002058063 ) ) ;
#4947 = CARTESIAN_POINT ( 'NONE',  ( 1.846138399168762101, -11.69739621335925328, 4.238866729160359448 ) ) ;
#4948 = CARTESIAN_POINT ( 'NONE',  ( 0.3308579732647032867, 10.76782854710826776, 8.558831104906948539 ) ) ;
#4949 = CARTESIAN_POINT ( 'NONE',  ( 0.4754618798421162973, 10.80499583390525586, -8.775436892860994931 ) ) ;
#4950 = CARTESIAN_POINT ( 'NONE',  ( 3.377929128793395019, 9.234024516648318581, 10.50432311212905923 ) ) ;
#4951 = AXIS2_PLACEMENT_3D ( 'NONE', #15564, #14231, #8498 ) ;
#4952 = CARTESIAN_POINT ( 'NONE',  ( 2.002547531651519996, 3.242439124566649511, 12.17374746633579541 ) ) ;
#4953 = ORIENTED_EDGE ( 'NONE', *, *, #14024, .T. ) ;
#4954 = PRODUCT_DEFINITION_SHAPE ( 'NONE', 'NONE',  #18916 ) ;
#4955 = EDGE_LOOP ( 'NONE', ( #3194, #9210, #15704, #1357 ) ) ;
#4956 = ORIENTED_EDGE ( 'NONE', *, *, #1753, .T. ) ;
#4957 = ADVANCED_FACE ( 'NONE', ( #7748, #13370 ), #479, .F. ) ;
#4958 = ORIENTED_EDGE ( 'NONE', *, *, #15956, .T. ) ;
#4959 = DIRECTION ( 'NONE',  ( 0.000000000000000000, 0.000000000000000000, 1.000000000000000000 ) ) ;
#4960 = CARTESIAN_POINT ( 'NONE',  ( 3.512766787571010241, 14.81029789862133583, -2.682019731918177996 ) ) ;
#4961 = CARTESIAN_POINT ( 'NONE',  ( 3.950837973638677170, 12.81214529934985080, -6.888253895133152227 ) ) ;
#4962 = AXIS2_PLACEMENT_3D ( 'NONE', #11330, #11518, #749 ) ;
#4963 = PLANE ( 'NONE',  #5345 ) ;
#4964 = VERTEX_POINT ( 'NONE', #17971 ) ;
#4965 = CARTESIAN_POINT ( 'NONE',  ( 0.2640320147533095074, 7.499999999999999112, -14.20017596028258744 ) ) ;
#4966 = EDGE_CURVE ( 'NONE', #18645, #2439, #11749, .T. ) ;
#4967 = CARTESIAN_POINT ( 'NONE',  ( 0.3150686449036101955, 13.11344473514187925, 4.099563462784696632 ) ) ;
#4968 = CARTESIAN_POINT ( 'NONE',  ( -0.3753471441346316051, 7.500000000000331291, -13.03644311608527850 ) ) ;
#4969 = CARTESIAN_POINT ( 'NONE',  ( 1.847412631396506022, -10.09191835241968427, 7.278870946904215877 ) ) ;
#4970 = FACE_OUTER_BOUND ( 'NONE', #2097, .T. ) ;
#4971 = CARTESIAN_POINT ( 'NONE',  ( 2.002547531651519996, -0.6781519942172617998, 12.57989064830759318 ) ) ;
#4972 = CARTESIAN_POINT ( 'NONE',  ( 2.179449471770337432, -4.500000000000000000, 0.000000000000000000 ) ) ;
#4973 = ORIENTED_EDGE ( 'NONE', *, *, #1340, .T. ) ;
#4975 = ORIENTED_EDGE ( 'NONE', *, *, #11491, .T. ) ;
#4974 = CARTESIAN_POINT ( 'NONE',  ( 3.074695600507183268, 7.366518011946177502, -13.70113613813200537 ) ) ;
#4976 = DIRECTION ( 'NONE',  ( -0.000000000000000000, 0.5000000000000003331, -0.8660254037844384856 ) ) ;
#4977 = VECTOR ( 'NONE', #15693, 1000.000000000000000 ) ;
#4978 = ORIENTED_EDGE ( 'NONE', *, *, #11215, .F. ) ;
#4979 = CARTESIAN_POINT ( 'NONE',  ( 1.846138399168762101, -4.238866729160323032, -11.69739621335926394 ) ) ;
#4980 = CARTESIAN_POINT ( 'NONE',  ( 1.149970134828444124, -6.907561563897677281, -11.99999999384792915 ) ) ;
#4981 = EDGE_CURVE ( 'NONE', #6753, #6997, #10463, .T. ) ;
#4982 = EDGE_LOOP ( 'NONE', ( #16888, #8730, #17424, #4423, #3792, #15660 ) ) ;
#4983 = LINE ( 'NONE', #10819, #8456 ) ;
#4984 = CARTESIAN_POINT ( 'NONE',  ( 0.3132642857406562342, -10.79548167658028213, -8.495623922778184678 ) ) ;
#4985 = CARTESIAN_POINT ( 'NONE',  ( 1.846138399168762101, -11.95493567637848109, -3.446241763653124401 ) ) ;
#4986 = CARTESIAN_POINT ( 'NONE',  ( 1.847380140988738484, 10.00162556679661741, -7.402792205948994564 ) ) ;
#4987 = EDGE_CURVE ( 'NONE', #2340, #10438, #6134, .T. ) ;
#4988 = AXIS2_PLACEMENT_3D ( 'NONE', #5741, #12922, #4327 ) ;
#4989 = CARTESIAN_POINT ( 'NONE',  ( 0.4754618798421167414, -11.68486377711971613, 7.564402563418431313 ) ) ;
#4990 = CARTESIAN_POINT ( 'NONE',  ( 3.950837973638668288, 0.000000000000000000, 0.000000000000000000 ) ) ;
#4992 = ORIENTED_EDGE ( 'NONE', *, *, #1919, .T. ) ;
#4991 = CARTESIAN_POINT ( 'NONE',  ( 2.636624412714237309, 14.14563173255211126, 7.605649742762011556 ) ) ;
#4993 = CARTESIAN_POINT ( 'NONE',  ( 2.636624412715138366, -11.10302021257964888, 11.60464335004044223 ) ) ;
#4994 = ORIENTED_EDGE ( 'NONE', *, *, #645, .T. ) ;
#4995 = CARTESIAN_POINT ( 'NONE',  ( 16.56753206892534891, 0.009369540855502130061, 0.001549402974393180796 ) ) ;
#4996 = CARTESIAN_POINT ( 'NONE',  ( 0.3720661004400037664, -13.34435358167255181, 3.575426119359132571 ) ) ;
#4997 = VERTEX_POINT ( 'NONE', #15605 ) ;
#4998 = ORIENTED_EDGE ( 'NONE', *, *, #18182, .F. ) ;
#4999 = CARTESIAN_POINT ( 'NONE',  ( 3.950837973638677170, 6.316429227969654114, -13.10350451991833687 ) ) ;
#5000 = EDGE_LOOP ( 'NONE', ( #2046, #9577, #2405, #6108 ) ) ;
#5001 = CARTESIAN_POINT ( 'NONE',  ( -2.179449471770337432, -4.500000000000000000, -6.000000000000000000 ) ) ;
#5002 = VERTEX_POINT ( 'NONE', #9860 ) ;
#5003 = CARTESIAN_POINT ( 'NONE',  ( 3.512766787570793969, 2.025881399556391127, 14.91422000116820179 ) ) ;
#5004 = EDGE_CURVE ( 'NONE', #16605, #7666, #18852, .T. ) ;
#5005 = AXIS2_PLACEMENT_3D ( 'NONE', #582, #289, #189 ) ;
#5006 = AXIS2_PLACEMENT_3D ( 'NONE', #14426, #5913, #11854 ) ;
#5007 = CARTESIAN_POINT ( 'NONE',  ( 16.56822296793089322, 0.002414375228568254022, -0.009847136207496285168 ) ) ;
#5008 = DIRECTION ( 'NONE',  ( 0.4246593920385850485, 0.1376957914266804250, -0.8948208031649687033 ) ) ;
#5009 = CARTESIAN_POINT ( 'NONE',  ( 0.3939822652208125886, 13.34132036472942318, -3.598529276937123544 ) ) ;
#5010 = ADVANCED_FACE ( 'NONE', ( #5475 ), #5744, .F. ) ;
#5011 = CARTESIAN_POINT ( 'NONE',  ( 2.123976203522053297, -1.531817366691861304, 15.54801196254786255 ) ) ;
#5012 = APPLICATION_PROTOCOL_DEFINITION ( 'draft international standard', 'automotive_design', 1998, #6076 ) ;
#5013 = CARTESIAN_POINT ( 'NONE',  ( 0.4754618798421162973, 7.564402563418637371, -11.68486377711958468 ) ) ;
#5014 = CARTESIAN_POINT ( 'NONE',  ( 2.697797270744668019, -3.226410068829341338, -12.89731672021093090 ) ) ;
#5015 = CARTESIAN_POINT ( 'NONE',  ( 2.697797270744666687, -8.537712152180933600, 10.19107313879054466 ) ) ;
#5016 = CARTESIAN_POINT ( 'NONE',  ( 0.4862570985993252548, 12.97920246947879441, 5.003653737315533867 ) ) ;
#5017 = CIRCLE ( 'NONE', #751, 5.000000000000004441 ) ;
#5018 = B_SPLINE_CURVE_WITH_KNOTS ( 'NONE', 3,
 ( #8945, #9517, #15525, #3686, #8096, #3598 ),
 .UNSPECIFIED., .F., .F.,
 ( 4, 2, 4 ),
 ( 2.239080928920849783E-18, 0.0002017457492448096685, 0.0004034914984896170601 ),
 .UNSPECIFIED. ) ;
#5019 = CARTESIAN_POINT ( 'NONE',  ( 2.002547531651519996, -10.57595306287296921, 6.845637710436153434 ) ) ;
#5020 = CARTESIAN_POINT ( 'NONE',  ( 16.56753206892534891, -0.001549402974394225099, -0.009369540855502527313 ) ) ;
#5021 = ORIENTED_EDGE ( 'NONE', *, *, #3206, .F. ) ;
#5022 = ORIENTED_EDGE ( 'NONE', *, *, #548, .F. ) ;
#5023 = ORIENTED_EDGE ( 'NONE', *, *, #9195, .T. ) ;
#5024 = EDGE_LOOP ( 'NONE', ( #18369, #18554, #12205, #13177 ) ) ;
#5025 = VERTEX_POINT ( 'NONE', #7018 ) ;
#5026 = CARTESIAN_POINT ( 'NONE',  ( 0.3150686449036065317, 11.20479228691397822, 7.951193823202440392 ) ) ;
#5027 = CARTESIAN_POINT ( 'NONE',  ( 5.934112841479999290, -7.500000000000002665, -16.97589560338757408 ) ) ;
#5028 = CIRCLE ( 'NONE', #17535, 5.000000000000004441 ) ;
#5029 = ADVANCED_FACE ( 'NONE', ( #17136 ), #5877, .F. ) ;
#5030 = CARTESIAN_POINT ( 'NONE',  ( 3.950837973638675393, 10.05648675950126325, 10.51028938476221342 ) ) ;
#5031 = CARTESIAN_POINT ( 'NONE',  ( 1.977436885026408353, 1.488549889122500192, -15.33079650480466860 ) ) ;
#5032 = VECTOR ( 'NONE', #2467, 1000.000000000000114 ) ;
#5033 = CARTESIAN_POINT ( 'NONE',  ( 2.123976203522053741, -3.347755036806012274, 15.26039569100259108 ) ) ;
#5034 = CARTESIAN_POINT ( 'NONE',  ( 0.4862570985993252548, 13.44146924561381162, 3.580942890621718888 ) ) ;
#5035 = CARTESIAN_POINT ( 'NONE',  ( -199.9999999999999716, -10.00000000000002665, 3.000000000000000000 ) ) ;
#5036 = CARTESIAN_POINT ( 'NONE',  ( 0.3170788640506440603, -7.952793437297492218, -11.20690911610912543 ) ) ;
#5037 = CARTESIAN_POINT ( 'NONE',  ( 3.664313757352971823, 2.831308606787245719, 13.97913389346634183 ) ) ;
#5038 = VERTEX_POINT ( 'NONE', #14360 ) ;
#5039 = ORIENTED_EDGE ( 'NONE', *, *, #11914, .T. ) ;
#5040 = EDGE_LOOP ( 'NONE', ( #18194, #6987, #15036, #3794 ) ) ;
#5041 = CIRCLE ( 'NONE', #12970, 16.06066017081991149 ) ;
#5042 = EDGE_LOOP ( 'NONE', ( #6703, #17230, #838, #5228 ) ) ;
#5043 = AXIS2_PLACEMENT_3D ( 'NONE', #3081, #4347, #10172 ) ;
#5044 = CARTESIAN_POINT ( 'NONE',  ( 4.755015822784811164, -4.336808689942017736E-16, 0.000000000000000000 ) ) ;
#5045 = CARTESIAN_POINT ( 'NONE',  ( 1.342453679581834924, 9.456403821038797730, 11.38190519890856933 ) ) ;
#5046 = CARTESIAN_POINT ( 'NONE',  ( 1.254255976358459757, 14.24071337840876694, -3.563435620217374478 ) ) ;
#5047 = FACE_OUTER_BOUND ( 'NONE', #7449, .T. ) ;
#5048 = FACE_OUTER_BOUND ( 'NONE', #12747, .T. ) ;
#5049 = VERTEX_POINT ( 'NONE', #12742 ) ;
#5050 = EDGE_CURVE ( 'NONE', #11395, #15844, #11233, .T. ) ;
#5051 = FACE_OUTER_BOUND ( 'NONE', #11840, .T. ) ;
#5052 = EDGE_CURVE ( 'NONE', #14724, #8524, #6613, .T. ) ;
#5053 = DIRECTION ( 'NONE',  ( -6.938893903907227392E-16, 0.000000000000000000, 1.000000000000000000 ) ) ;
#5054 = EDGE_CURVE ( 'NONE', #14675, #10843, #5917, .T. ) ;
#5055 = CARTESIAN_POINT ( 'NONE',  ( 0.2197594725759999534, 7.500000000000027534, -13.03330426732994951 ) ) ;
#5056 = CARTESIAN_POINT ( 'NONE',  ( 16.56872352241294521, 0.009382111268606257298, -0.004564908236400254740 ) ) ;
#5057 =( BOUNDED_SURFACE ( )  B_SPLINE_SURFACE ( 3, 1, ( 
 ( #12595, #5510 ),
 ( #5336, #11363 ),
 ( #11180, #10107 ),
 ( #3909, #9731 ) ),
 .UNSPECIFIED., .F., .F., .T. ) 
 B_SPLINE_SURFACE_WITH_KNOTS ( ( 4, 4 ),
 ( 2, 2 ),
 ( 0.000000000000000000, 1.000000000000000000 ),
 ( 0.000000000000000000, 1.000000000000000000 ),
 .UNSPECIFIED. ) 
 GEOMETRIC_REPRESENTATION_ITEM ( )  RATIONAL_B_SPLINE_SURFACE ( (
 ( 1.000000000000000000, 1.000000000000000000),
 ( 0.9593108457356467333, 0.9995965569486454649),
 ( 0.9593108457356467333, 0.9995965569486454649),
 ( 1.000000000000000000, 1.000000000000000000) ) ) 
 REPRESENTATION_ITEM ( '' )  SURFACE ( )  );
#5058 = CARTESIAN_POINT ( 'NONE',  ( -27.32408120756002035, 15.00000000000000000, 3.000000000000000000 ) ) ;
#5059 = CARTESIAN_POINT ( 'NONE',  ( -7.000000000000000000, 0.000000000000000000, 8.000000000000000000 ) ) ;
#5060 = CARTESIAN_POINT ( 'NONE',  ( 0.3148213771069354738, 13.13560149728606419, -4.026433757158845772 ) ) ;
#5061 = CIRCLE ( 'NONE', #790, 16.06066017081991149 ) ;
#5062 = AXIS2_PLACEMENT_3D ( 'NONE', #18421, #585, #5149 ) ;
#5063 = ORIENTED_EDGE ( 'NONE', *, *, #10218, .T. ) ;
#5065 = ORIENTED_EDGE ( 'NONE', *, *, #4690, .F. ) ;
#5064 = CARTESIAN_POINT ( 'NONE',  ( 2.123976203522053741, -11.67822624909933005, 10.37815841598487765 ) ) ;
#5066 = CARTESIAN_POINT ( 'NONE',  ( 1.560000000000000053, -0.8660254037844384856, -1.500000000000000000 ) ) ;
#5067 = ORIENTED_EDGE ( 'NONE', *, *, #16170, .T. ) ;
#5068 = CARTESIAN_POINT ( 'NONE',  ( 0.3720661004400040439, 11.58636699658215541, 7.524064345033506740 ) ) ;
#5069 = AXIS2_PLACEMENT_3D ( 'NONE', #9801, #13931, #3621 ) ;
#5070 = CARTESIAN_POINT ( 'NONE',  ( -2.482385025457884087, -7.500000000000001776, -13.17615586950463857 ) ) ;
#5071 = B_SPLINE_CURVE_WITH_KNOTS ( 'NONE', 3,
 ( #8810, #16468, #12066, #14638, #15018, #1938 ),
 .UNSPECIFIED., .F., .F.,
 ( 4, 2, 4 ),
 ( 0.000000000000000000, 0.0001828790815886940750, 0.0003657581631773881500 ),
 .UNSPECIFIED. ) ;
#5072 = ORIENTED_EDGE ( 'NONE', *, *, #6420, .F. ) ;
#5073 = DIRECTION ( 'NONE',  ( -1.000000000000000000, 1.224646799147353454E-16, 0.000000000000000000 ) ) ;
#5074 = CARTESIAN_POINT ( 'NONE',  ( -194.9999999999999716, 9.999999999999973355, 11.00000000000000000 ) ) ;
#5075 = CARTESIAN_POINT ( 'NONE',  ( 2.636624412714237309, 15.80357026013209953, 2.862162146984226663 ) ) ;
#5076 = CARTESIAN_POINT ( 'NONE',  ( 20.00000000000000000, -2.500000000000000444, -17.00000000000000000 ) ) ;
#5077 = EDGE_CURVE ( 'NONE', #18014, #2316, #16619, .T. ) ;
#5078 = ADVANCED_FACE ( 'NONE', ( #15890 ), #4784, .F. ) ;
#5079 = FILL_AREA_STYLE_COLOUR ( '', #12704 ) ;
#5080 = CARTESIAN_POINT ( 'NONE',  ( 1.861628059977341598, 12.44564375541077617, 0.5393144007390715533 ) ) ;
#5081 = MECHANICAL_DESIGN_GEOMETRIC_PRESENTATION_REPRESENTATION (  '', ( #16981 ), #1102 ) ;
#5082 = CARTESIAN_POINT ( 'NONE',  ( -54.57590088527786065, 9.999999999999973355, 3.000000000000000000 ) ) ;
#5084 = ORIENTED_EDGE ( 'NONE', *, *, #8168, .F. ) ;
#5083 = CARTESIAN_POINT ( 'NONE',  ( 3.377929128793395908, -12.84367544717939680, 5.536064832134110603 ) ) ;
#5085 = DIRECTION ( 'NONE',  ( 0.000000000000000000, 0.000000000000000000, 1.000000000000000000 ) ) ;
#5086 = B_SPLINE_CURVE_WITH_KNOTS ( 'NONE', 3,
 ( #424, #16389, #3276, #12088, #7407, #17921 ),
 .UNSPECIFIED., .F., .F.,
 ( 4, 2, 4 ),
 ( 4.336808689942017736E-19, 0.0001828790815886937498, 0.0003657581631773870658 ),
 .UNSPECIFIED. ) ;
#5087 = VERTEX_POINT ( 'NONE', #2780 ) ;
#5088 = CARTESIAN_POINT ( 'NONE',  ( 0.8740764193767950330, -14.27348595579787371, -0.8420116711623154560 ) ) ;
#5089 = CARTESIAN_POINT ( 'NONE',  ( 16.56822296793089322, 0.005339139727952666586, -0.008619100080559792543 ) ) ;
#5090 = ORIENTED_EDGE ( 'NONE', *, *, #3408, .T. ) ;
#5091 = ORIENTED_EDGE ( 'NONE', *, *, #6885, .F. ) ;
#5092 = LINE ( 'NONE', #797, #10325 ) ;
#5093 = CIRCLE ( 'NONE', #15766, 4.750000000000000000 ) ;
#5094 = APPLICATION_CONTEXT ( 'automotive_design' ) ;
#5095 = DIRECTION ( 'NONE',  ( -1.000000000000000000, -0.000000000000000000, -0.000000000000000000 ) ) ;
#5096 = B_SPLINE_CURVE_WITH_KNOTS ( 'NONE', 3,
 ( #1537, #16259, #14715, #16057 ),
 .UNSPECIFIED., .F., .F.,
 ( 4, 4 ),
 ( 2.168404344971008868E-17, 0.003005512676784848763 ),
 .UNSPECIFIED. ) ;
#5097 = VERTEX_POINT ( 'NONE', #7210 ) ;
#5098 = VECTOR ( 'NONE', #1181, 1000.000000000000000 ) ;
#5099 = VECTOR ( 'NONE', #6375, 1000.000000000000114 ) ;
#5100 = FACE_OUTER_BOUND ( 'NONE', #16616, .T. ) ;
#5101 = ADVANCED_FACE ( 'NONE', ( #4330 ), #6743, .F. ) ;
#5102 = B_SPLINE_CURVE_WITH_KNOTS ( 'NONE', 3,
 ( #12500, #9363, #6777, #5237, #6860, #12684, #3712, #848, #18511, #5421, #8211, #756, #15195 ),
 .UNSPECIFIED., .F., .F.,
 ( 4, 3, 3, 3, 4 ),
 ( 2.453269466693398698E-18, 0.0002299804304191500187, 0.0004599608082120258223, 0.0006467586077648020170, 0.0008336169836825994828 ),
 .UNSPECIFIED. ) ;
#5103 = DIRECTION ( 'NONE',  ( -1.000000000000000000, 0.000000000000000000, 0.000000000000000000 ) ) ;
#5104 = CARTESIAN_POINT ( 'NONE',  ( 0.3132642857406530146, 13.21852905223344088, -3.740125687984594993 ) ) ;
#5105 = EDGE_CURVE ( 'NONE', #5495, #12765, #1555, .T. ) ;
#5106 = VECTOR ( 'NONE', #1546, 1000.000000000000000 ) ;
#5107 = EDGE_CURVE ( 'NONE', #13762, #8587, #15031, .T. ) ;
#5108 = CARTESIAN_POINT ( 'NONE',  ( 16.57210152137263393, -0.01402404281923042353, -0.003862718596009419997 ) ) ;
#5109 = PRODUCT_CONTEXT ( 'NONE', #8042, 'mechanical' ) ;
#5110 = CARTESIAN_POINT ( 'NONE',  ( 1.845755665166725068, 10.33920510797153369, -6.920419570228236950 ) ) ;
#5111 = CARTESIAN_POINT ( 'NONE',  ( 1.254255976358046087, 5.487601330835574664, -13.61551404021248857 ) ) ;
#5112 = CIRCLE ( 'NONE', #14261, 14.54644660717763927 ) ;
#5113 = CARTESIAN_POINT ( 'NONE',  ( 16.56782317627811096, 0.0003415813796014688375, 0.009814734722106369796 ) ) ;
#5114 = CARTESIAN_POINT ( 'NONE',  ( 0.4862570985993235340, -12.97920246947883172, 5.003653737315437944 ) ) ;
#5115 = CARTESIAN_POINT ( 'NONE',  ( 3.943463214271659518E-15, -16.60000000000000142, 22.91316734529526045 ) ) ;
#5116 = CARTESIAN_POINT ( 'NONE',  ( 8.522092701127531811, -5.397361180353174248, 4.388629235579559307 ) ) ;
#5117 = VERTEX_POINT ( 'NONE', #14736 ) ;
#5118 = EDGE_CURVE ( 'NONE', #7783, #12607, #18145, .T. ) ;
#5119 = VERTEX_POINT ( 'NONE', #224 ) ;
#5120 = VERTEX_POINT ( 'NONE', #11786 ) ;
#5121 = VERTEX_POINT ( 'NONE', #4420 ) ;
#5122 = AXIS2_PLACEMENT_3D ( 'NONE', #9223, #17833, #2238 ) ;
#5123 = EDGE_CURVE ( 'NONE', #15077, #5247, #8371, .T. ) ;
#5124 = CARTESIAN_POINT ( 'NONE',  ( 1.959283090834838870, -9.750336807931205385, 7.909254450748972154 ) ) ;
#5125 = CARTESIAN_POINT ( 'NONE',  ( 1.876079424475004975, -7.500000000000001776, -15.16033210860608804 ) ) ;
#5126 = B_SPLINE_CURVE_WITH_KNOTS ( 'NONE', 3,
 ( #16687, #3590, #18208, #8089, #13899, #3770 ),
 .UNSPECIFIED., .F., .F.,
 ( 4, 2, 4 ),
 ( 3.144186300207962859E-18, 0.0002017457492448081777, 0.0004034914984896132112 ),
 .UNSPECIFIED. ) ;
#5127 = VERTEX_POINT ( 'NONE', #4619 ) ;
#5128 = DIRECTION ( 'NONE',  ( 0.000000000000000000, 0.000000000000000000, 1.000000000000000000 ) ) ;
#5129 = CARTESIAN_POINT ( 'NONE',  ( 8.522092701127531811, 6.489356537178190720, 2.505958102592644288 ) ) ;
#5130 = CARTESIAN_POINT ( 'NONE',  ( 15.00000000000000711, -40.00000000000000000, 6.000000000000000000 ) ) ;
#5131 = CARTESIAN_POINT ( 'NONE',  ( 0.000000000000000000, 0.000000000000000000, 10.00000000000000000 ) ) ;
#5132 = CARTESIAN_POINT ( 'NONE',  ( -30.00000000000000355, -12.50000000000000178, 0.000000000000000000 ) ) ;
#5133 = CARTESIAN_POINT ( 'NONE',  ( 0.3170788640506440603, -4.100430649997872656, -13.11595226728161911 ) ) ;
#5134 = EDGE_CURVE ( 'NONE', #2099, #7234, #17530, .T. ) ;
#5135 = ORIENTED_EDGE ( 'NONE', *, *, #12903, .F. ) ;
#5136 = ORIENTED_EDGE ( 'NONE', *, *, #10427, .T. ) ;
#5137 = EDGE_CURVE ( 'NONE', #6376, #6854, #1751, .T. ) ;
#5138 = ORIENTED_EDGE ( 'NONE', *, *, #2143, .T. ) ;
#5139 = ORIENTED_EDGE ( 'NONE', *, *, #14975, .T. ) ;
#5140 = FACE_OUTER_BOUND ( 'NONE', #527, .T. ) ;
#5141 = VECTOR ( 'NONE', #13606, 1000.000000000000000 ) ;
#5142 = DIRECTION ( 'NONE',  ( 0.000000000000000000, 0.000000000000000000, 1.000000000000000000 ) ) ;
#5143 = DIRECTION ( 'NONE',  ( 0.7635533937278216055, 0.3966532189476633663, -0.5095610256143844330 ) ) ;
#5144 = CARTESIAN_POINT ( 'NONE',  ( 3.950837973638676281, 10.05648675950141602, -10.51028938476206953 ) ) ;
#5145 = LINE ( 'NONE', #3898, #14518 ) ;
#5146 = ORIENTED_EDGE ( 'NONE', *, *, #3989, .F. ) ;
#5147 = CARTESIAN_POINT ( 'NONE',  ( -6.154177238272306560, 7.499999999999997335, -12.51861270110133262 ) ) ;
#5148 = CARTESIAN_POINT ( 'NONE',  ( 2.002547531651519996, -7.942910686618240845, 9.778737580845669797 ) ) ;
#5149 = DIRECTION ( 'NONE',  ( -1.000000000000000000, 0.000000000000000000, 0.000000000000000000 ) ) ;
#5150 = CARTESIAN_POINT ( 'NONE',  ( 3.377929128793395908, -7.136734442940921852, 12.02809354424098665 ) ) ;
#5151 = CARTESIAN_POINT ( 'NONE',  ( 25.00000000000000000, -2.500000000000000444, -17.00000000000000000 ) ) ;
#5152 = DIRECTION ( 'NONE',  ( -1.000000000000000000, -0.000000000000000000, -0.000000000000000000 ) ) ;
#5153 = ORIENTED_EDGE ( 'NONE', *, *, #13866, .T. ) ;
#5155 = VERTEX_POINT ( 'NONE', #11683 ) ;
#5154 = CARTESIAN_POINT ( 'NONE',  ( 1.254009781011991453, -9.426200207651724838, -11.25324419414228494 ) ) ;
#5156 = ADVANCED_FACE ( 'NONE', ( #7690 ), #3434, .F. ) ;
#5157 = EDGE_CURVE ( 'NONE', #5049, #6997, #14777, .T. ) ;
#5158 = EDGE_CURVE ( 'NONE', #5753, #16885, #1034, .T. ) ;
#5159 = B_SPLINE_CURVE_WITH_KNOTS ( 'NONE', 3,
 ( #10699, #9163, #10893, #7841 ),
 .UNSPECIFIED., .F., .F.,
 ( 4, 4 ),
 ( 0.000000000000000000, 0.002004993803842800969 ),
 .UNSPECIFIED. ) ;
#5160 = AXIS2_PLACEMENT_3D ( 'NONE', #10028, #15862, #1917 ) ;
#5161 = CARTESIAN_POINT ( 'NONE',  ( 1.846822687350018866, -0.2922081769261017925, 12.43915556955403723 ) ) ;
#5162 = ORIENTED_EDGE ( 'NONE', *, *, #9337, .F. ) ;
#5163 = CARTESIAN_POINT ( 'NONE',  ( 1.846955891736120181, -4.094751675596620011, -11.74973605926568077 ) ) ;
#5164 = CARTESIAN_POINT ( 'NONE',  ( -0.4829358362134061333, -7.500000000000000888, -14.27056707468136665 ) ) ;
#5165 =( BOUNDED_SURFACE ( )  B_SPLINE_SURFACE ( 3, 1, ( 
 ( #14101, #1007 ),
 ( #5408, #9790 ),
 ( #4167, #2521 ),
 ( #7129, #12946 ) ),
 .UNSPECIFIED., .F., .F., .T. ) 
 B_SPLINE_SURFACE_WITH_KNOTS ( ( 4, 4 ),
 ( 2, 2 ),
 ( 0.000000000000000000, 1.000000000000000000 ),
 ( 0.000000000000000000, 1.000000000000000000 ),
 .UNSPECIFIED. ) 
 GEOMETRIC_REPRESENTATION_ITEM ( )  RATIONAL_B_SPLINE_SURFACE ( (
 ( 1.000000000000000000, 1.000000000000000000),
 ( 0.7792777138730160313, 0.9689936506012927220),
 ( 0.7792777138730160313, 0.9689936506012927220),
 ( 1.000000000000000000, 1.000000000000000000) ) ) 
 REPRESENTATION_ITEM ( '' )  SURFACE ( )  );
#5166 = ORIENTED_EDGE ( 'NONE', *, *, #11622, .T. ) ;
#5167 = CYLINDRICAL_SURFACE ( 'NONE', #17229, 5.000000000000000888 ) ;
#5168 = CARTESIAN_POINT ( 'NONE',  ( 0.4862570985993235340, -7.559321496869506163, 11.67702470553362559 ) ) ;
#5169 = DIRECTION ( 'NONE',  ( 0.000000000000000000, 0.000000000000000000, 1.000000000000000000 ) ) ;
#5170 = CARTESIAN_POINT ( 'NONE',  ( 6.538348415311010520, -2.500000000000000444, -12.00000000000000000 ) ) ;
#5171 = ADVANCED_FACE ( 'NONE', ( #16179 ), #1464, .F. ) ;
#5172 = CIRCLE ( 'NONE', #5770, 5.000000000000000000 ) ;
#5173 = CIRCLE ( 'NONE', #9454, 5.315148208181397216 ) ;
#5174 = AXIS2_PLACEMENT_3D ( 'NONE', #9830, #15662, #8410 ) ;
#5175 = FACE_OUTER_BOUND ( 'NONE', #12880, .T. ) ;
#5176 = CARTESIAN_POINT ( 'NONE',  ( 15.00000000000000711, -19.99999999999999645, 6.000000000000000000 ) ) ;
#5178 = ORIENTED_EDGE ( 'NONE', *, *, #7354, .T. ) ;
#5177 = CARTESIAN_POINT ( 'NONE',  ( -194.9999999999999716, 14.99999999999997513, 3.000000000000002665 ) ) ;
#5179 = CARTESIAN_POINT ( 'NONE',  ( -194.9999999999999716, -15.00000000000002665, 3.000000000000002665 ) ) ;
#5180 = VERTEX_POINT ( 'NONE', #13208 ) ;
#5181 = CARTESIAN_POINT ( 'NONE',  ( 0.4862570985993235340, 8.769551628660735787, 10.79774104611376373 ) ) ;
#5182 = CARTESIAN_POINT ( 'NONE',  ( 1.846138399168762989, -4.238866729160486457, 11.69739621335920710 ) ) ;
#5183 = ORIENTED_EDGE ( 'NONE', *, *, #824, .T. ) ;
#5184 = ORIENTED_EDGE ( 'NONE', *, *, #5354, .T. ) ;
#5185 = CARTESIAN_POINT ( 'NONE',  ( 3.950837973638675393, -13.10350451991835818, -6.316429227969608817 ) ) ;
#5186 = EDGE_CURVE ( 'NONE', #10401, #1657, #2042, .T. ) ;
#5187 = DIRECTION ( 'NONE',  ( -1.000000000000000000, -0.000000000000000000, -0.000000000000000000 ) ) ;
#5188 = ORIENTED_EDGE ( 'NONE', *, *, #10541, .T. ) ;
#5189 = CARTESIAN_POINT ( 'NONE',  ( 3.074695600507260984, -10.75417554975707013, 11.23985886659431621 ) ) ;
#5190 = CARTESIAN_POINT ( 'NONE',  ( 1.845756295923353996, 6.920504327368345976, -10.33914852636097592 ) ) ;
#5191 = CYLINDRICAL_SURFACE ( 'NONE', #6126, 7.000000000000000000 ) ;
#5192 = DIRECTION ( 'NONE',  ( 0.000000000000000000, 0.000000000000000000, 1.000000000000000000 ) ) ;
#5193 = CARTESIAN_POINT ( 'NONE',  ( 0.4385251269669947494, 13.39302348765813910, -3.577373010348575910 ) ) ;
#5194 = EDGE_CURVE ( 'NONE', #471, #8324, #8201, .T. ) ;
#5195 = SURFACE_SIDE_STYLE ('',( #2236 ) ) ;
#5196 = SHAPE_DEFINITION_REPRESENTATION ( #6483, #4478 ) ;
#5197 = CARTESIAN_POINT ( 'NONE',  ( 16.56753206892534891, 0.001421777558676785977, 0.009389754735541558373 ) ) ;
#5198 = CARTESIAN_POINT ( 'NONE',  ( 2.636624412715137478, -2.862162146983530775, 15.80357026013314048 ) ) ;
#5199 = ORIENTED_EDGE ( 'NONE', *, *, #9706, .T. ) ;
#5200 = SHAPE_REPRESENTATION ( 'BR-823', ( #18727, #5675, #533, #14252, #6015, #10916, #3243, #2935, #8151, #18813, #12127, #12717, #10597, #15463, #13652 ), #4491 ) ;
#5201 =( BOUNDED_SURFACE ( )  B_SPLINE_SURFACE ( 3, 1, ( 
 ( #13109, #14725 ),
 ( #13296, #5546 ),
 ( #18842, #5931 ),
 ( #5736, #17407 ) ),
 .UNSPECIFIED., .F., .F., .T. ) 
 B_SPLINE_SURFACE_WITH_KNOTS ( ( 4, 4 ),
 ( 2, 2 ),
 ( 0.000000000000000000, 1.000000000000000000 ),
 ( 0.000000000000000000, 1.000000000000000000 ),
 .UNSPECIFIED. ) 
 GEOMETRIC_REPRESENTATION_ITEM ( )  RATIONAL_B_SPLINE_SURFACE ( (
 ( 1.000000000000000000, 1.000000000000000000),
 ( 0.9593108457356467333, 0.9995965569486454649),
 ( 0.9593108457356467333, 0.9995965569486454649),
 ( 1.000000000000000000, 1.000000000000000000) ) ) 
 REPRESENTATION_ITEM ( '' )  SURFACE ( )  );
#5202 = CARTESIAN_POINT ( 'NONE',  ( 1.847412631396503357, 7.348689888531986014, -10.04119192206678512 ) ) ;
#5203 = AXIS2_PLACEMENT_3D ( 'NONE', #3255, #9100, #14057 ) ;
#5204 = CARTESIAN_POINT ( 'NONE',  ( 2.705023505549863039, 13.27418276223636084, -0.8488853074253436271 ) ) ;
#5205 = CARTESIAN_POINT ( 'NONE',  ( 15.00000000000000711, -19.99999999999999645, 3.000000000000000000 ) ) ;
#5206 = CARTESIAN_POINT ( 'NONE',  ( 16.56679352167444819, 0.004277682826582259769, -0.008252760440870513317 ) ) ;
#5207 = ADVANCED_FACE ( 'NONE', ( #3740, #6530 ), #5267, .T. ) ;
#5208 = EDGE_LOOP ( 'NONE', ( #8729, #18264, #18857, #4076 ) ) ;
#5209 = ORIENTED_EDGE ( 'NONE', *, *, #6980, .T. ) ;
#5210 = EDGE_CURVE ( 'NONE', #7697, #4027, #16399, .T. ) ;
#5211 = EDGE_CURVE ( 'NONE', #9296, #3540, #2218, .T. ) ;
#5212 = ORIENTED_EDGE ( 'NONE', *, *, #14729, .T. ) ;
#5213 = EDGE_LOOP ( 'NONE', ( #7112, #2747, #5872, #1234 ) ) ;
#5214 = DIRECTION ( 'NONE',  ( 0.7561779333270773895, 0.2350349629540228469, -0.6106991889125047424 ) ) ;
#5215 = EDGE_CURVE ( 'NONE', #13145, #698, #14787, .T. ) ;
#5216 = CARTESIAN_POINT ( 'NONE',  ( -1.823557580623804908, -7.500000000000002665, -15.12114310604040845 ) ) ;
#5217 = CARTESIAN_POINT ( 'NONE',  ( 1.959212340397962882, -12.53706137681889210, -0.6675998551413099280 ) ) ;
#5218 = CARTESIAN_POINT ( 'NONE',  ( 0.8740779401508861346, -7.708543377337782054, 12.04241618260063618 ) ) ;
#5219 = ADVANCED_FACE ( 'NONE', ( #16839 ), #9485, .T. ) ;
#5220 = CARTESIAN_POINT ( 'NONE',  ( -194.9999999999999716, -25.00000000000003197, 3.000000000000000000 ) ) ;
#5221 = CARTESIAN_POINT ( 'NONE',  ( 2.636624412714237309, 14.14563173255211126, 7.605649742762011556 ) ) ;
#5222 = AXIS2_PLACEMENT_3D ( 'NONE', #13476, #592, #12153 ) ;
#5223 = CARTESIAN_POINT ( 'NONE',  ( 2.002547531651519996, -12.17374746633575988, -3.242439124566779185 ) ) ;
#5224 = CARTESIAN_POINT ( 'NONE',  ( -199.9999999999999716, 4.999999999999973355, 6.000000000000000000 ) ) ;
#5225 = CARTESIAN_POINT ( 'NONE',  ( -1.389456752619696367, -44.31487138727242581, 6.000000000000000000 ) ) ;
#5226 = ORIENTED_EDGE ( 'NONE', *, *, #4263, .F. ) ;
#5227 = ORIENTED_EDGE ( 'NONE', *, *, #15690, .F. ) ;
#5228 = ORIENTED_EDGE ( 'NONE', *, *, #4718, .F. ) ;
#5229 = ORIENTED_EDGE ( 'NONE', *, *, #3588, .F. ) ;
#5230 = LINE ( 'NONE', #18862, #15334 ) ;
#5231 = CARTESIAN_POINT ( 'NONE',  ( 16.58200780006414732, 0.01041078477704048856, 0.004047297414159084679 ) ) ;
#5232 = VECTOR ( 'NONE', #17908, 1000.000000000000114 ) ;
#5233 = CARTESIAN_POINT ( 'NONE',  ( 2.353870697619111052, -12.05847592522640355, -4.720869121224258613 ) ) ;
#5234 = CARTESIAN_POINT ( 'NONE',  ( -66.35602477868047799, 9.999999999999973355, 3.000000000000002665 ) ) ;
#5235 = DIRECTION ( 'NONE',  ( 1.000000000000000000, 1.298018465182616140E-16, 0.000000000000000000 ) ) ;
#5236 = ORIENTED_EDGE ( 'NONE', *, *, #6491, .T. ) ;
#5237 = CARTESIAN_POINT ( 'NONE',  ( 1.847168016377981781, 10.17509564929258836, 7.161712042621497076 ) ) ;
#5238 = B_SPLINE_CURVE_WITH_KNOTS ( 'NONE', 3,
 ( #14140, #12896, #8239, #5359, #18719, #12988, #18820, #14336, #2562, #11568, #8328, #17389, #10029 ),
 .UNSPECIFIED., .F., .F.,
 ( 4, 3, 3, 3, 4 ),
 ( 4.670885906470169154E-18, 0.0002299780670421044384, 0.0004599561239687884940, 0.0006896788984287876298, 0.0009194956271626387621 ),
 .UNSPECIFIED. ) ;
#5239 = ADVANCED_FACE ( 'NONE', ( #3558 ), #515, .F. ) ;
#5240 = CARTESIAN_POINT ( 'NONE',  ( 2.002547531651519996, 0.6781519942171739812, 12.57989064830759851 ) ) ;
#5241 = CARTESIAN_POINT ( 'NONE',  ( -1.213280723412490714, 7.499999999999931610, -13.07603167631473440 ) ) ;
#5242 = CARTESIAN_POINT ( 'NONE',  ( 1.918921323896324971, -6.832782632379298171, -10.48468902844559913 ) ) ;
#5243 = CARTESIAN_POINT ( 'NONE',  ( 2.949999999999999734, 0.000000000000000000, 2.500000000000000000 ) ) ;
#5244 = EDGE_CURVE ( 'NONE', #12234, #3343, #18505, .T. ) ;
#5245 = CARTESIAN_POINT ( 'NONE',  ( 0.3151928476913548605, 13.06671852871095574, -4.245853234426248513 ) ) ;
#5246 = CARTESIAN_POINT ( 'NONE',  ( 25.00000000000000000, -7.500000000000000888, -16.99999999999999645 ) ) ;
#5247 = VERTEX_POINT ( 'NONE', #13782 ) ;
#5249 = ORIENTED_EDGE ( 'NONE', *, *, #648, .T. ) ;
#5248 = CARTESIAN_POINT ( 'NONE',  ( 2.369999999999999662, 0.000000000000000000, 0.000000000000000000 ) ) ;
#5250 = DIRECTION ( 'NONE',  ( -0.000000000000000000, -0.000000000000000000, 1.000000000000000000 ) ) ;
#5251 = CIRCLE ( 'NONE', #2791, 5.315148208181396328 ) ;
#5252 = CARTESIAN_POINT ( 'NONE',  ( 1.560000000000000053, 0.000000000000000000, 2.999999999999998668 ) ) ;
#5253 = ORIENTED_EDGE ( 'NONE', *, *, #6704, .F. ) ;
#5254 = CARTESIAN_POINT ( 'NONE',  ( 2.636624412715138366, -15.91454522070249311, -2.161493821597819665 ) ) ;
#5255 = DIRECTION ( 'NONE',  ( 1.000000000000000000, 0.000000000000000000, 0.000000000000000000 ) ) ;
#5256 = ORIENTED_EDGE ( 'NONE', *, *, #4095, .T. ) ;
#5257 = CARTESIAN_POINT ( 'NONE',  ( 1.846822687350024417, -7.547953575784189795, 9.891732594446548177 ) ) ;
#5258 = CARTESIAN_POINT ( 'NONE',  ( 0.4384471787762834749, 13.84291427302851574, -0.7363690479466810102 ) ) ;
#5259 = DIRECTION ( 'NONE',  ( 0.000000000000000000, 0.000000000000000000, -1.000000000000000000 ) ) ;
#5260 = CARTESIAN_POINT ( 'NONE',  ( 1.846138399168762101, 9.815003036200520725, -7.646096044339786069 ) ) ;
#5261 = EDGE_CURVE ( 'NONE', #17548, #7381, #12172, .T. ) ;
#5262 = ADVANCED_FACE ( 'NONE', ( #16568 ), #8674, .F. ) ;
#5263 = CARTESIAN_POINT ( 'NONE',  ( 8.438534575730034959, 6.862570336891075762, 0.2320579683290369954 ) ) ;
#5264 = EDGE_CURVE ( 'NONE', #11365, #14216, #12347, .T. ) ;
#5265 = CARTESIAN_POINT ( 'NONE',  ( -59.99999999999997158, -25.00000000000000711, 0.000000000000000000 ) ) ;
#5266 = DIRECTION ( 'NONE',  ( 0.000000000000000000, 0.000000000000000000, -1.000000000000000000 ) ) ;
#5268 = ORIENTED_EDGE ( 'NONE', *, *, #9337, .T. ) ;
#5267 = PLANE ( 'NONE',  #3171 ) ;
#5269 = DIRECTION ( 'NONE',  ( -0.7561779333270775005, 0.2350349629540185170, 0.6106991889125065187 ) ) ;
#5270 = AXIS2_PLACEMENT_3D ( 'NONE', #7177, #5288, #18822 ) ;
#5271 = CARTESIAN_POINT ( 'NONE',  ( 0.3137051932979792457, -10.83767969834796929, -8.442169467526971616 ) ) ;
#5272 = CARTESIAN_POINT ( 'NONE',  ( 1.846138399168762101, 4.238866729160568170, -11.69739621335917690 ) ) ;
#5273 =( BOUNDED_SURFACE ( )  B_SPLINE_SURFACE ( 3, 1, ( 
 ( #4884, #15099 ),
 ( #587, #3533 ),
 ( #12325, #2821 ),
 ( #8577, #15641 ) ),
 .UNSPECIFIED., .F., .F., .T. ) 
 B_SPLINE_SURFACE_WITH_KNOTS ( ( 4, 4 ),
 ( 2, 2 ),
 ( 0.000000000000000000, 1.000000000000000000 ),
 ( 0.000000000000000000, 1.000000000000000000 ),
 .UNSPECIFIED. ) 
 GEOMETRIC_REPRESENTATION_ITEM ( )  RATIONAL_B_SPLINE_SURFACE ( (
 ( 1.000000000000000000, 1.000000000000000000),
 ( 0.7792777138730160313, 0.9689936506012927220),
 ( 0.7792777138730160313, 0.9689936506012927220),
 ( 1.000000000000000000, 1.000000000000000000) ) ) 
 REPRESENTATION_ITEM ( '' )  SURFACE ( )  );
#5274 = ORIENTED_EDGE ( 'NONE', *, *, #2400, .T. ) ;
#5275 = VERTEX_POINT ( 'NONE', #16932 ) ;
#5276 = CARTESIAN_POINT ( 'NONE',  ( 0.4862570985993235340, -8.769551628660812170, 10.79774104611370333 ) ) ;
#5277 = CARTESIAN_POINT ( 'NONE',  ( 3.353306896162455697, -7.069984850384722463, -12.02594772223104869 ) ) ;
#5278 = ORIENTED_EDGE ( 'NONE', *, *, #7573, .F. ) ;
#5279 = CARTESIAN_POINT ( 'NONE',  ( 0.3308579732647030647, -4.812490080619291177, 12.88563776947744088 ) ) ;
#5280 =( NAMED_UNIT ( * ) PLANE_ANGLE_UNIT ( ) SI_UNIT ( $, .RADIAN. ) );
#5281 = CARTESIAN_POINT ( 'NONE',  ( 16.56782317627811096, 0.003357783021327236019, -0.009228812961909608689 ) ) ;
#5282 = CARTESIAN_POINT ( 'NONE',  ( 2.636624412714756005, -2.161493821597335607, 15.91454522070219113 ) ) ;
#5283 = CARTESIAN_POINT ( 'NONE',  ( 0.3939875929385635023, -7.545068896001288827, 11.57636969881031241 ) ) ;
#5284 = ADVANCED_FACE ( 'NONE', ( #8153 ), #10274, .T. ) ;
#5285 = AXIS2_PLACEMENT_3D ( 'NONE', #8439, #2331, #2594 ) ;
#5286 = EDGE_CURVE ( 'NONE', #15079, #12032, #8864, .T. ) ;
#5287 = ADVANCED_FACE ( 'NONE', ( #2668 ), #6996, .T. ) ;
#5288 = DIRECTION ( 'NONE',  ( -1.000000000000000000, -0.000000000000000000, -0.000000000000000000 ) ) ;
#5289 = APPLICATION_PROTOCOL_DEFINITION ( 'draft international standard', 'automotive_design', 1998, #8042 ) ;
#5290 = EDGE_CURVE ( 'NONE', #18780, #18879, #12118, .T. ) ;
#5291 = DIRECTION ( 'NONE',  ( 1.000000000000000000, 0.000000000000000000, 0.000000000000000000 ) ) ;
#5292 = CARTESIAN_POINT ( 'NONE',  ( 0.3151926232592482946, -13.04305446098359056, 4.318679262939574492 ) ) ;
#5293 = CARTESIAN_POINT ( 'NONE',  ( 0.000000000000000000, 0.8660254037844389297, -1.500000000000000000 ) ) ;
#5294 = LINE ( 'NONE', #2691, #15474 ) ;
#5295 = CARTESIAN_POINT ( 'NONE',  ( 3.353306896162453477, -12.02594772223101494, 7.069984850384768649 ) ) ;
#5296 = CARTESIAN_POINT ( 'NONE',  ( 0.4754618798421162973, 8.775436892861113947, 10.80499583390515994 ) ) ;
#5297 = ORIENTED_EDGE ( 'NONE', *, *, #13444, .F. ) ;
#5298 = AXIS2_PLACEMENT_3D ( 'NONE', #2334, #7105, #903 ) ;
#5299 = EDGE_LOOP ( 'NONE', ( #6978, #9402, #3266, #13239 ) ) ;
#5300 = ORIENTED_EDGE ( 'NONE', *, *, #9989, .F. ) ;
#5301 = ORIENTED_EDGE ( 'NONE', *, *, #14124, .F. ) ;
#5302 = CARTESIAN_POINT ( 'NONE',  ( 0.3151928476913548050, 11.11539186930587242, 8.075547435846990751 ) ) ;
#5303 = CARTESIAN_POINT ( 'NONE',  ( 0.7623231285407791047, -7.500000000000001776, -14.39641017501655718 ) ) ;
#5304 = CARTESIAN_POINT ( 'NONE',  ( 0.4862570985993235340, 13.89016912371017476, 0.7479633556562934604 ) ) ;
#5305 = CARTESIAN_POINT ( 'NONE',  ( 3.512766787570778870, -6.535475144496882827, -13.55823433651953636 ) ) ;
#5306 =( BOUNDED_SURFACE ( )  B_SPLINE_SURFACE ( 3, 1, ( 
 ( #13466, #13669 ),
 ( #383, #12145 ),
 ( #6207, #9171 ),
 ( #7753, #13562 ) ),
 .UNSPECIFIED., .F., .F., .T. ) 
 B_SPLINE_SURFACE_WITH_KNOTS ( ( 4, 4 ),
 ( 2, 2 ),
 ( 0.000000000000000000, 1.000000000000000000 ),
 ( 0.000000000000000000, 1.000000000000000000 ),
 .UNSPECIFIED. ) 
 GEOMETRIC_REPRESENTATION_ITEM ( )  RATIONAL_B_SPLINE_SURFACE ( (
 ( 1.000000000000000000, 1.000000000000000000),
 ( 0.9933953342250436691, 0.8357391271907733676),
 ( 0.9933953342250436691, 0.8357391271907733676),
 ( 1.000000000000000000, 1.000000000000000000) ) ) 
 REPRESENTATION_ITEM ( '' )  SURFACE ( )  );
#5307 = AXIS2_PLACEMENT_3D ( 'NONE', #3306, #9148, #10388 ) ;
#5308 = LINE ( 'NONE', #12945, #17319 ) ;
#5309 = AXIS2_PLACEMENT_3D ( 'NONE', #11179, #5599, #1027 ) ;
#5310 = EDGE_CURVE ( 'NONE', #17659, #492, #2926, .T. ) ;
#5311 = CARTESIAN_POINT ( 'NONE',  ( 0.3137051932979792457, 7.698472063774471685, 11.37800749014133928 ) ) ;
#5312 = FACE_OUTER_BOUND ( 'NONE', #10962, .T. ) ;
#5313 = DIRECTION ( 'NONE',  ( 1.000000000000000000, 0.000000000000000000, 0.000000000000000000 ) ) ;
#5314 = ORIENTED_EDGE ( 'NONE', *, *, #11516, .F. ) ;
#5315 = VERTEX_POINT ( 'NONE', #17031 ) ;
#5316 = ORIENTED_EDGE ( 'NONE', *, *, #7146, .F. ) ;
#5317 = B_SPLINE_CURVE_WITH_KNOTS ( 'NONE', 3,
 ( #18371, #16667, #9405, #5277, #3373, #798 ),
 .UNSPECIFIED., .F., .F.,
 ( 4, 2, 4 ),
 ( 0.000000000000000000, 0.001500839035891551789, 0.003001678071783103578 ),
 .UNSPECIFIED. ) ;
#5318 = ORIENTED_EDGE ( 'NONE', *, *, #9306, .T. ) ;
#5319 = VECTOR ( 'NONE', #16971, 1000.000000000000000 ) ;
#5320 = CARTESIAN_POINT ( 'NONE',  ( 12.00000000000000711, -19.99999999999999645, 8.000000000000000000 ) ) ;
#5321 = EDGE_CURVE ( 'NONE', #16055, #796, #14063, .T. ) ;
#5322 = DIRECTION ( 'NONE',  ( 0.000000000000000000, 0.8660254037844384856, -0.5000000000000004441 ) ) ;
#5323 = CARTESIAN_POINT ( 'NONE',  ( 0.3170788640506440603, -13.74111462631963398, -0.1533108587037582682 ) ) ;
#5324 = B_SPLINE_CURVE_WITH_KNOTS ( 'NONE', 3,
 ( #2020, #4786, #13383, #17887, #7761, #10622 ),
 .UNSPECIFIED., .F., .F.,
 ( 4, 2, 4 ),
 ( 9.215718466126787689E-19, 0.001657017934710630505, 0.003314035869421260144 ),
 .UNSPECIFIED. ) ;
#5325 = FACE_OUTER_BOUND ( 'NONE', #2633, .T. ) ;
#5326 = CARTESIAN_POINT ( 'NONE',  ( 1.560000000000000053, -0.8660254037844384856, 1.500000000000000000 ) ) ;
#5327 = ORIENTED_EDGE ( 'NONE', *, *, #17881, .F. ) ;
#5328 = CARTESIAN_POINT ( 'NONE',  ( 0.4754618798421162973, 8.775436892861270266, -10.80499583390503382 ) ) ;
#5329 = AXIS2_PLACEMENT_3D ( 'NONE', #10143, #7290, #8994 ) ;
#5330 = CARTESIAN_POINT ( 'NONE',  ( 1.846138399168762101, -11.69739621335919111, -4.238866729160527314 ) ) ;
#5331 = CIRCLE ( 'NONE', #9601, 1.000000000000000000 ) ;
#5332 = CARTESIAN_POINT ( 'NONE',  ( 6.499600586847153139, 2.601338725571119337, -12.00000000000000000 ) ) ;
#5333 = CARTESIAN_POINT ( 'NONE',  ( 12.00000000000000711, -15.99999999999999645, 8.000000000000000000 ) ) ;
#5334 = CARTESIAN_POINT ( 'NONE',  ( -66.35602477868047799, -15.00000000000001066, 3.000000000000002665 ) ) ;
#5335 = PLANE ( 'NONE',  #7776 ) ;
#5336 = CARTESIAN_POINT ( 'NONE',  ( 16.56679352167444819, 0.006526964904752955397, 0.006618561353599231728 ) ) ;
#5337 = CARTESIAN_POINT ( 'NONE',  ( 0.8740764193769091639, -3.609949042658162188, -13.83508774436024957 ) ) ;
#5338 = ORIENTED_EDGE ( 'NONE', *, *, #7986, .F. ) ;
#5339 = AXIS2_PLACEMENT_3D ( 'NONE', #3760, #16584, #15418 ) ;
#5340 = CIRCLE ( 'NONE', #16015, 2.750000000000000000 ) ;
#5341 = ADVANCED_BREP_SHAPE_REPRESENTATION ( '', ( #3708, #2030 ), #2329 ) ;
#5343 = ORIENTED_EDGE ( 'NONE', *, *, #2076, .T. ) ;
#5342 = CARTESIAN_POINT ( 'NONE',  ( 0.3058872367615230181, 0.6080468242580958638, 13.72992299905060243 ) ) ;
#5344 = CARTESIAN_POINT ( 'NONE',  ( 16.58200780006414732, 0.008650561019685530303, -0.007066318000004736047 ) ) ;
#5345 = AXIS2_PLACEMENT_3D ( 'NONE', #3126, #3225, #7943 ) ;
#5346 = DIRECTION ( 'NONE',  ( -1.000000000000000000, -0.000000000000000000, -0.000000000000000000 ) ) ;
#5347 = EDGE_CURVE ( 'NONE', #3169, #1518, #825, .T. ) ;
#5348 = ORIENTED_EDGE ( 'NONE', *, *, #18195, .F. ) ;
#5349 = DIRECTION ( 'NONE',  ( 0.000000000000000000, 0.000000000000000000, -1.000000000000000000 ) ) ;
#5350 = CARTESIAN_POINT ( 'NONE',  ( -6.340401435272320363, -2.969608215370683979, -11.99999999980919618 ) ) ;
#5351 = DIRECTION ( 'NONE',  ( -0.7635533937278214944, 0.6071939193889607234, -0.2197766120036399873 ) ) ;
#5352 = EDGE_LOOP ( 'NONE', ( #654, #10815 ) ) ;
#5353 = CARTESIAN_POINT ( 'NONE',  ( 0.8740764193772003754, 13.83508774436055511, -3.609949042658134211 ) ) ;
#5354 = EDGE_CURVE ( 'NONE', #10558, #5097, #12905, .T. ) ;
#5355 = CARTESIAN_POINT ( 'NONE',  ( -30.00000000000000355, -12.50000000000000178, 6.000000000000000000 ) ) ;
#5356 = AXIS2_PLACEMENT_3D ( 'NONE', #10757, #11997, #17831 ) ;
#5357 = CARTESIAN_POINT ( 'NONE',  ( 3.074695600508759785, 15.30693405987895694, 2.772091048737280072 ) ) ;
#5358 = TOROIDAL_SURFACE ( 'NONE', #12676, 5.000000000000005329, 5.000000000000000000 ) ;
#5359 = CARTESIAN_POINT ( 'NONE',  ( 0.3148213771069381384, -12.99360322443199678, -4.463459503829131592 ) ) ;
#5360 = CARTESIAN_POINT ( 'NONE',  ( -32.49999999999999289, -12.50000000000000178, 6.000000000000000000 ) ) ;
#5361 = DIRECTION ( 'NONE',  ( 0.000000000000000000, 0.000000000000000000, -1.000000000000000000 ) ) ;
#5362 = CARTESIAN_POINT ( 'NONE',  ( 0.000000000000000000, 6.799999999999999822, 1.500000000000000000 ) ) ;
#5364 = ORIENTED_EDGE ( 'NONE', *, *, #10049, .F. ) ;
#5363 = DIRECTION ( 'NONE',  ( -1.000000000000000000, -0.000000000000000000, -0.000000000000000000 ) ) ;
#5365 = CARTESIAN_POINT ( 'NONE',  ( 2.747332970342022840, -7.289199830147006232, -14.63517873738954655 ) ) ;
#5366 = VECTOR ( 'NONE', #3710, 1000.000000000000000 ) ;
#5367 = CARTESIAN_POINT ( 'NONE',  ( -6.538348415311010520, 2.499999999999998668, -12.00000000000000000 ) ) ;
#5368 = CARTESIAN_POINT ( 'NONE',  ( 0.8740764193764966050, 11.05257066464512405, 9.070946295053792241 ) ) ;
#5369 = AXIS2_PLACEMENT_3D ( 'NONE', #9493, #11119, #7983 ) ;
#5370 = ADVANCED_FACE ( 'NONE', ( #12619, #2761 ), #14433, .T. ) ;
#5371 = ORIENTED_EDGE ( 'NONE', *, *, #13574, .T. ) ;
#5372 = CARTESIAN_POINT ( 'NONE',  ( 2.002547531651519996, -0.6781519942172617998, 12.57989064830759318 ) ) ;
#5373 = DIRECTION ( 'NONE',  ( -1.000000000000000000, -0.000000000000000000, -0.000000000000000000 ) ) ;
#5374 = ORIENTED_EDGE ( 'NONE', *, *, #269, .F. ) ;
#5375 = DIRECTION ( 'NONE',  ( 1.000000000000000000, 0.000000000000000000, 0.000000000000000000 ) ) ;
#5376 = CARTESIAN_POINT ( 'NONE',  ( 1.562796894703937678, 0.000000000000000000, 0.000000000000000000 ) ) ;
#5377 = CARTESIAN_POINT ( 'NONE',  ( 0.3151928478948589074, -0.0001388664988634735829, -13.73922860964089487 ) ) ;
#5378 = PLANE ( 'NONE',  #4794 ) ;
#5379 = UNCERTAINTY_MEASURE_WITH_UNIT (LENGTH_MEASURE( 1.000000000000000082E-05 ), #992, 'distance_accuracy_value', 'NONE');
#5380 = AXIS2_PLACEMENT_3D ( 'NONE', #335, #13226, #6163 ) ;
#5381 = SHAPE_DEFINITION_REPRESENTATION ( #6165, #5200 ) ;
#5382 =( GEOMETRIC_REPRESENTATION_CONTEXT ( 3 ) GLOBAL_UNCERTAINTY_ASSIGNED_CONTEXT ( ( #7478 ) ) GLOBAL_UNIT_ASSIGNED_CONTEXT ( ( #15328, #3581, #16496 ) ) REPRESENTATION_CONTEXT ( 'NONE', 'WORKASPACE' ) );
#5383 =( LENGTH_UNIT ( ) NAMED_UNIT ( * ) SI_UNIT ( .MILLI., .METRE. ) );
#5384 = DIRECTION ( 'NONE',  ( 0.000000000000000000, 1.000000000000000000, 0.000000000000000000 ) ) ;
#5385 = CARTESIAN_POINT ( 'NONE',  ( 0.3151930723728423867, -13.09040889075573411, 4.172946285306520231 ) ) ;
#5386 =( BOUNDED_SURFACE ( )  B_SPLINE_SURFACE ( 3, 1, ( 
 ( #11748, #13266 ),
 ( #17683, #10315 ),
 ( #8874, #11845 ),
 ( #6201, #9165 ) ),
 .UNSPECIFIED., .F., .F., .T. ) 
 B_SPLINE_SURFACE_WITH_KNOTS ( ( 4, 4 ),
 ( 2, 2 ),
 ( 0.000000000000000000, 1.000000000000000000 ),
 ( 0.000000000000000000, 1.000000000000000000 ),
 .UNSPECIFIED. ) 
 GEOMETRIC_REPRESENTATION_ITEM ( )  RATIONAL_B_SPLINE_SURFACE ( (
 ( 1.000000000000000000, 1.000000000000000000),
 ( 0.9593108457356467333, 0.9995965569486454649),
 ( 0.9593108457356467333, 0.9995965569486454649),
 ( 1.000000000000000000, 1.000000000000000000) ) ) 
 REPRESENTATION_ITEM ( '' )  SURFACE ( )  );
#5387 = CARTESIAN_POINT ( 'NONE',  ( 3.377929128793396796, -1.296196549818846355, -13.92579934231097560 ) ) ;
#5388 = CARTESIAN_POINT ( 'NONE',  ( 0.3170788640506440603, 11.20690911610915208, -7.952793437297452250 ) ) ;
#5389 = CARTESIAN_POINT ( 'NONE',  ( 1.560000000000000053, 0.000000000000000000, 0.000000000000000000 ) ) ;
#5390 = CIRCLE ( 'NONE', #7858, 5.000000000000000888 ) ;
#5391 = CARTESIAN_POINT ( 'NONE',  ( 3.664313757352973600, -12.42002390572631221, 7.012524439851453906 ) ) ;
#5392 = PRESENTATION_STYLE_ASSIGNMENT (( #18481 ) ) ;
#5393 = ORIENTED_EDGE ( 'NONE', *, *, #15943, .F. ) ;
#5394 = ADVANCED_FACE ( 'NONE', ( #9942 ), #6125, .F. ) ;
#5395 = EDGE_CURVE ( 'NONE', #2148, #12310, #16407, .T. ) ;
#5396 = VERTEX_POINT ( 'NONE', #4022 ) ;
#5397 = VERTEX_POINT ( 'NONE', #5727 ) ;
#5398 = ORIENTED_EDGE ( 'NONE', *, *, #4135, .T. ) ;
#5399 = AXIS2_PLACEMENT_3D ( 'NONE', #6409, #7851, #4685 ) ;
#5400 = CARTESIAN_POINT ( 'NONE',  ( 0.3137051932979757485, 12.91601973349276733, -4.679953077377353665 ) ) ;
#5401 = DIRECTION ( 'NONE',  ( -1.000000000000000000, 0.000000000000000000, 0.000000000000000000 ) ) ;
#5402 = CIRCLE ( 'NONE', #16088, 1.500000000000000000 ) ;
#5403 = FACE_OUTER_BOUND ( 'NONE', #6720, .T. ) ;
#5404 = CARTESIAN_POINT ( 'NONE',  ( 3.950837973638676281, 13.10350451991840615, 6.316429227969512894 ) ) ;
#5405 = VECTOR ( 'NONE', #5269, 1000.000000000000114 ) ;
#5406 = DIRECTION ( 'NONE',  ( 0.000000000000000000, 0.000000000000000000, -1.000000000000000000 ) ) ;
#5407 = CARTESIAN_POINT ( 'NONE',  ( 1.104287921197080512E-14, -7.013167318348350499, 22.41316734529519650 ) ) ;
#5408 = CARTESIAN_POINT ( 'NONE',  ( 16.57210152137263393, 0.01402404281923039231, 0.003862718596009517575 ) ) ;
#5409 = CARTESIAN_POINT ( 'NONE',  ( -61.35602477868047799, -10.00000000000000888, 6.000000000000000000 ) ) ;
#5410 = ORIENTED_EDGE ( 'NONE', *, *, #6617, .T. ) ;
#5411 = ORIENTED_EDGE ( 'NONE', *, *, #490, .T. ) ;
#5412 = ORIENTED_EDGE ( 'NONE', *, *, #12668, .T. ) ;
#5413 = ORIENTED_EDGE ( 'NONE', *, *, #4711, .T. ) ;
#5414 = CARTESIAN_POINT ( 'NONE',  ( 2.949999999999999734, 0.000000000000000000, 0.000000000000000000 ) ) ;
#5415 = EDGE_CURVE ( 'NONE', #16059, #15061, #7895, .T. ) ;
#5416 = CARTESIAN_POINT ( 'NONE',  ( 16.56782317627811096, 0.006045301465876368185, -0.007739510688079533247 ) ) ;
#5417 = CARTESIAN_POINT ( 'NONE',  ( 0.4754618798421162973, -8.775436892861190330, 10.80499583390509954 ) ) ;
#5418 = DIRECTION ( 'NONE',  ( -1.000000000000000000, 0.000000000000000000, 0.000000000000000000 ) ) ;
#5419 = EDGE_CURVE ( 'NONE', #5896, #1187, #3254, .T. ) ;
#5420 = VERTEX_POINT ( 'NONE', #2573 ) ;
#5421 = CARTESIAN_POINT ( 'NONE',  ( 1.847034903785825577, 9.929438108952146180, 7.498375632854650696 ) ) ;
#5422 = CARTESIAN_POINT ( 'NONE',  ( 1.562796894703937678, 6.799999999999999822, 1.500000000000000000 ) ) ;
#5423 = CARTESIAN_POINT ( 'NONE',  ( 4.153045036174358273, 5.656186534233338392, -12.00000000830655367 ) ) ;
#5424 = DIRECTION ( 'NONE',  ( 0.000000000000000000, 0.000000000000000000, -1.000000000000000000 ) ) ;
#5425 = EDGE_CURVE ( 'NONE', #15939, #4248, #5683, .T. ) ;
#5426 = CIRCLE ( 'NONE', #10306, 5.000000000000000888 ) ;
#5427 = DIRECTION ( 'NONE',  ( 0.000000000000000000, 0.000000000000000000, 1.000000000000000000 ) ) ;
#5428 = CARTESIAN_POINT ( 'NONE',  ( 0.3137051932979809665, 13.20008686438111312, -3.805684345189650042 ) ) ;
#5429 = DIRECTION ( 'NONE',  ( 0.000000000000000000, 0.000000000000000000, 1.000000000000000000 ) ) ;
#5430 = CARTESIAN_POINT ( 'NONE',  ( 1.846138399168762989, -3.446241763653083101, 11.95493567637849530 ) ) ;
#5431 = ORIENTED_EDGE ( 'NONE', *, *, #9873, .F. ) ;
#5432 = VERTEX_POINT ( 'NONE', #4120 ) ;
#5433 = CARTESIAN_POINT ( 'NONE',  ( 3.950837973638668288, 0.000000000000000000, 0.000000000000000000 ) ) ;
#5434 = PRODUCT_DEFINITION ( 'UNKNOWN', '', #13558, #3503 ) ;
#5435 = EDGE_CURVE ( 'NONE', #15699, #15587, #8163, .T. ) ;
#5436 = CARTESIAN_POINT ( 'NONE',  ( 0.3095370825347233956, -10.84046130709064393, 8.444334731363969837 ) ) ;
#5437 = EDGE_LOOP ( 'NONE', ( #14926, #11910, #8580, #82 ) ) ;
#5438 = CARTESIAN_POINT ( 'NONE',  ( 2.636624412714242194, 14.46769361191244485, 6.973567714906650394 ) ) ;
#5439 = EDGE_CURVE ( 'NONE', #5705, #10186, #7549, .T. ) ;
#5440 = EDGE_CURVE ( 'NONE', #1445, #4455, #16775, .T. ) ;
#5441 = CARTESIAN_POINT ( 'NONE',  ( -6.259160902251362124, -7.500000000000261124, -12.42139992667873649 ) ) ;
#5442 = CARTESIAN_POINT ( 'NONE',  ( 3.950837973638676281, 2.591948120962007884, -14.31366178983250670 ) ) ;
#5443 = ORIENTED_EDGE ( 'NONE', *, *, #4445, .F. ) ;
#5444 = CARTESIAN_POINT ( 'NONE',  ( 2.636624412715137922, -15.91454522070252153, 2.161493821597598508 ) ) ;
#5445 = CARTESIAN_POINT ( 'NONE',  ( -4.000000000000000888, 17.00000000000000000, 8.000000000000000000 ) ) ;
#5446 = CARTESIAN_POINT ( 'NONE',  ( 0.4862570985993235340, -13.89016912371016943, -0.7479633556563904939 ) ) ;
#5447 = CARTESIAN_POINT ( 'NONE',  ( 3.512766787570810401, -2.025881399556277440, -14.91422000116817159 ) ) ;
#5448 = CARTESIAN_POINT ( 'NONE',  ( 15.00000000000000711, -18.99999999999999645, 8.000000000000000000 ) ) ;
#5449 = EDGE_CURVE ( 'NONE', #9813, #14004, #5921, .T. ) ;
#5450 = FILL_AREA_STYLE_COLOUR ( '', #8753 ) ;
#5451 = CARTESIAN_POINT ( 'NONE',  ( 2.636624412716902288, 7.605649742760546950, -14.14563173255513995 ) ) ;
#5452 = CARTESIAN_POINT ( 'NONE',  ( 2.123976203522053297, 3.347755036805901252, 15.26039569100260884 ) ) ;
#5454 = ORIENTED_EDGE ( 'NONE', *, *, #4040, .T. ) ;
#5453 = DIRECTION ( 'NONE',  ( -1.000000000000000000, -0.000000000000000000, -0.000000000000000000 ) ) ;
#5455 = CARTESIAN_POINT ( 'NONE',  ( 0.3308579732647004001, 0.5950689966506276241, -13.74211098745268345 ) ) ;
#5456 = CARTESIAN_POINT ( 'NONE',  ( 0.3939822652208130327, -0.7002900021918908591, 13.80035637018651862 ) ) ;
#5457 = ORIENTED_EDGE ( 'NONE', *, *, #11252, .T. ) ;
#5458 = DIRECTION ( 'NONE',  ( -1.000000000000000000, -0.000000000000000000, -0.000000000000000000 ) ) ;
#5459 = CARTESIAN_POINT ( 'NONE',  ( 0.3137051932979792457, -13.20008686438103140, -3.805684345189927154 ) ) ;
#5460 = ORIENTED_EDGE ( 'NONE', *, *, #13691, .T. ) ;
#5461 = CARTESIAN_POINT ( 'NONE',  ( 0.4754618798421167414, 0.7484603771386338922, -13.89949764182681768 ) ) ;
#5462 = DIRECTION ( 'NONE',  ( 0.000000000000000000, -1.000000000000000000, 0.000000000000000000 ) ) ;
#5463 = CIRCLE ( 'NONE', #6402, 2.100000000000000977 ) ;
#5464 = CARTESIAN_POINT ( 'NONE',  ( 0.3151930723728477157, -11.16020735774772277, 8.013866567350856229 ) ) ;
#5465 = CARTESIAN_POINT ( 'NONE',  ( 3.512766787570727356, 6.535475144497194577, -13.55823433651945464 ) ) ;
#5466 = EDGE_LOOP ( 'NONE', ( #2341, #1496, #6560 ) ) ;
#5467 = EDGE_CURVE ( 'NONE', #3343, #12234, #10605, .T. ) ;
#5468 = ITEM_DEFINED_TRANSFORMATION ( 'NONE', 'NONE', #3243,  #2030 ) ;
#5469 = STYLED_ITEM ( 'NONE', ( #6732 ), #3619 ) ;
#5470 = FILL_AREA_STYLE_COLOUR ( '', #7544 ) ;
#5471 = CARTESIAN_POINT ( 'NONE',  ( 0.4384471787762820871, -13.39294437382615399, -3.577367180593688634 ) ) ;
#5472 = EDGE_CURVE ( 'NONE', #3568, #2148, #17696, .T. ) ;
#5473 = CARTESIAN_POINT ( 'NONE',  ( 1.861628059977344263, -0.5393144007391119654, 12.44564375541076728 ) ) ;
#5474 = CARTESIAN_POINT ( 'NONE',  ( 3.950837973638668288, 0.000000000000000000, 0.000000000000000000 ) ) ;
#5475 = FACE_OUTER_BOUND ( 'NONE', #13295, .T. ) ;
#5476 = DIRECTION ( 'NONE',  ( 0.000000000000000000, 0.000000000000000000, 1.000000000000000000 ) ) ;
#5477 = ORIENTED_EDGE ( 'NONE', *, *, #10518, .F. ) ;
#5478 = ORIENTED_EDGE ( 'NONE', *, *, #1586, .T. ) ;
#5479 = ORIENTED_EDGE ( 'NONE', *, *, #18361, .F. ) ;
#5480 = ORIENTED_EDGE ( 'NONE', *, *, #12072, .T. ) ;
#5481 = ORIENTED_EDGE ( 'NONE', *, *, #13945, .F. ) ;
#5482 = CARTESIAN_POINT ( 'NONE',  ( -66.35602477868047799, 9.999999999999973355, 3.000000000000002665 ) ) ;
#5483 = CARTESIAN_POINT ( 'NONE',  ( 2.636624412716062960, 6.973567714909310489, -14.46769361191320868 ) ) ;
#5484 = FACE_OUTER_BOUND ( 'NONE', #16147, .T. ) ;
#5485 = CARTESIAN_POINT ( 'NONE',  ( 1.846138399168762101, 6.971848976711011225, 10.30487220521572667 ) ) ;
#5486 = EDGE_CURVE ( 'NONE', #10168, #14610, #4216, .T. ) ;
#5487 = EDGE_CURVE ( 'NONE', #16059, #9890, #2345, .T. ) ;
#5488 = CARTESIAN_POINT ( 'NONE',  ( 3.377929128793398128, -5.536064832134078628, -12.84367544717941456 ) ) ;
#5489 = EDGE_CURVE ( 'NONE', #12673, #16909, #6319, .T. ) ;
#5490 = CARTESIAN_POINT ( 'NONE',  ( 2.123976203522053741, 3.347755036806118856, -15.26039569100256266 ) ) ;
#5491 = CARTESIAN_POINT ( 'NONE',  ( 0.3142014840576517476, -13.17932813834297434, 3.879477880151391833 ) ) ;
#5492 = CARTESIAN_POINT ( 'NONE',  ( 1.861706995891674099, -12.44571539481144384, 0.5394761475745415424 ) ) ;
#5493 = ORIENTED_EDGE ( 'NONE', *, *, #3866, .F. ) ;
#5494 = B_SPLINE_CURVE_WITH_KNOTS ( 'NONE', 3,
 ( #8716, #5737, #18843, #10147, #14541, #12734, #4132, #8618, #1456, #12915, #4410, #7295, #4033 ),
 .UNSPECIFIED., .F., .F.,
 ( 4, 3, 3, 3, 4 ),
 ( 1.734723475976807094E-18, 0.0002299780670421052245, 0.0004599561239687887651, 0.0006896788984287890393, 0.0009194956271626402800 ),
 .UNSPECIFIED. ) ;
#5495 = VERTEX_POINT ( 'NONE', #8888 ) ;
#5496 = ORIENTED_EDGE ( 'NONE', *, *, #566, .F. ) ;
#5497 = ORIENTED_EDGE ( 'NONE', *, *, #1804, .T. ) ;
#5498 = EDGE_CURVE ( 'NONE', #18306, #11651, #5577, .T. ) ;
#5499 = CARTESIAN_POINT ( 'NONE',  ( 0.000000000000000000, 0.000000000000000000, 0.000000000000000000 ) ) ;
#5500 = CARTESIAN_POINT ( 'NONE',  ( 3.950837973638675393, -10.51028938476210328, -10.05648675950137871 ) ) ;
#5501 = CARTESIAN_POINT ( 'NONE',  ( 0.3058872367615230181, 4.821066432589326212, 12.87003593440630311 ) ) ;
#5502 = CARTESIAN_POINT ( 'NONE',  ( 2.320520222536567090, 11.60169517779319293, 10.64885284334832960 ) ) ;
#5503 = DIRECTION ( 'NONE',  ( 0.000000000000000000, 0.000000000000000000, 1.000000000000000000 ) ) ;
#5504 = VERTEX_POINT ( 'NONE', #2951 ) ;
#5505 = DIRECTION ( 'NONE',  ( -1.000000000000000000, -0.000000000000000000, -0.000000000000000000 ) ) ;
#5506 = CARTESIAN_POINT ( 'NONE',  ( 3.074695600507708182, 10.75417554975745205, 11.23985886659407463 ) ) ;
#5507 = CARTESIAN_POINT ( 'NONE',  ( 6.234321419756527760, 7.499999999999999112, -16.99999999998787104 ) ) ;
#5508 = CARTESIAN_POINT ( 'NONE',  ( 2.636624412714236865, 0.000000000000000000, 0.000000000000000000 ) ) ;
#5509 = FACE_OUTER_BOUND ( 'NONE', #7867, .T. ) ;
#5510 = CARTESIAN_POINT ( 'NONE',  ( 0.3095370825347224519, -11.38092634279622928, -7.700448427571997989 ) ) ;
#5511 = ADVANCED_FACE ( 'NONE', ( #8799 ), #4598, .F. ) ;
#5512 = FACE_OUTER_BOUND ( 'NONE', #7162, .T. ) ;
#5513 = ORIENTED_EDGE ( 'NONE', *, *, #3086, .T. ) ;
#5514 = EDGE_CURVE ( 'NONE', #799, #15883, #8701, .T. ) ;
#5516 = EDGE_LOOP ( 'NONE', ( #17627, #865, #11953, #1682 ) ) ;
#5515 = CARTESIAN_POINT ( 'NONE',  ( 0.3137051932979792457, -13.73004976592201842, -0.4596302728641207813 ) ) ;
#5517 = CARTESIAN_POINT ( 'NONE',  ( 0.3939875929385661668, 4.930599594904554017, 12.90850834464102270 ) ) ;
#5518 = VERTEX_POINT ( 'NONE', #7471 ) ;
#5519 = VECTOR ( 'NONE', #5794, 1000.000000000000000 ) ;
#5520 = CARTESIAN_POINT ( 'NONE',  ( 0.4754618798421162973, -10.80499583390518836, 8.775436892861078420 ) ) ;
#5521 = EDGE_CURVE ( 'NONE', #1137, #1087, #6032, .T. ) ;
#5522 = ORIENTED_EDGE ( 'NONE', *, *, #5547, .F. ) ;
#5523 = CARTESIAN_POINT ( 'NONE',  ( -66.35602477868049220, 9.999999999999973355, 5.999999999999999112 ) ) ;
#5524 = CARTESIAN_POINT ( 'NONE',  ( -6.273991221456290290, -3.109390318170350387, -12.00000000063440098 ) ) ;
#5525 = DIRECTION ( 'NONE',  ( 0.000000000000000000, 0.000000000000000000, 1.000000000000000000 ) ) ;
#5526 = ORIENTED_EDGE ( 'NONE', *, *, #6144, .F. ) ;
#5527 = CARTESIAN_POINT ( 'NONE',  ( 1.846613052777652531, -3.520031056876387954, 11.93415846513960332 ) ) ;
#5528 = CARTESIAN_POINT ( 'NONE',  ( 0.3145734862173232838, -3.953068532979906458, -13.15783074029282673 ) ) ;
#5529 = CARTESIAN_POINT ( 'NONE',  ( 1.846138399168762101, 12.43476674860266584, -0.4167076046095982700 ) ) ;
#5530 = CARTESIAN_POINT ( 'NONE',  ( 0.000000000000000000, 0.000000000000000000, -1.500000000000000000 ) ) ;
#5531 = B_SPLINE_CURVE_WITH_KNOTS ( 'NONE', 3,
 ( #7209, #5842, #18851, #5743 ),
 .UNSPECIFIED., .F., .F.,
 ( 4, 4 ),
 ( 1.927807806696441531E-17, 0.003005512676784856570 ),
 .UNSPECIFIED. ) ;
#5532 = CARTESIAN_POINT ( 'NONE',  ( 1.104287921197080512E-14, -7.013167318348350499, 22.41316734529519650 ) ) ;
#5533 = CARTESIAN_POINT ( 'NONE',  ( 1.560000000000000053, 0.8660254037844389297, -1.500000000000000000 ) ) ;
#5534 = CIRCLE ( 'NONE', #18667, 2.750000000000000000 ) ;
#5535 = CARTESIAN_POINT ( 'NONE',  ( 3.686287386450715076E-15, -27.00000000000000000, 27.11316734529526329 ) ) ;
#5537 = EDGE_LOOP ( 'NONE', ( #17841, #16364, #7550, #5084 ) ) ;
#5536 = CARTESIAN_POINT ( 'NONE',  ( 3.950837973638676281, -14.41405733518061716, 1.958075594453740687 ) ) ;
#5538 = CARTESIAN_POINT ( 'NONE',  ( 1.560000000000000053, 0.000000000000000000, -1.499999999999999556 ) ) ;
#5539 = CARTESIAN_POINT ( 'NONE',  ( 0.3137051932979792457, -0.4596302728640728752, 13.73004976592201842 ) ) ;
#5540 = EDGE_CURVE ( 'NONE', #6435, #7502, #1538, .T. ) ;
#5541 = EDGE_LOOP ( 'NONE', ( #1297, #12434, #16868, #17434 ) ) ;
#5542 = CARTESIAN_POINT ( 'NONE',  ( 0.3151928476913556376, 4.245457024760402653, -13.06684726503522320 ) ) ;
#5543 = CARTESIAN_POINT ( 'NONE',  ( 0.3151928479966099039, 0.07658992383256929548, -13.73922861026898623 ) ) ;
#5544 = B_SPLINE_CURVE_WITH_KNOTS ( 'NONE', 3,
 ( #1100, #12764, #18588, #5492, #17157, #4068 ),
 .UNSPECIFIED., .F., .F.,
 ( 4, 2, 4 ),
 ( 5.421010862427522170E-19, 0.0001825746017570591031, 0.0003651492035141176641 ),
 .UNSPECIFIED. ) ;
#5545 = ORIENTED_EDGE ( 'NONE', *, *, #1586, .F. ) ;
#5546 = CARTESIAN_POINT ( 'NONE',  ( 0.3170788640506441158, -4.100430649998053845, 13.11595226728156405 ) ) ;
#5547 = EDGE_CURVE ( 'NONE', #13860, #5420, #6044, .T. ) ;
#5548 = LINE ( 'NONE', #2231, #17998 ) ;
#5549 = DIRECTION ( 'NONE',  ( -0.000000000000000000, 0.000000000000000000, -1.000000000000000000 ) ) ;
#5550 = FACE_OUTER_BOUND ( 'NONE', #18681, .T. ) ;
#5551 = CARTESIAN_POINT ( 'NONE',  ( 3.950837973638668288, 0.000000000000000000, 0.000000000000000000 ) ) ;
#5552 = EDGE_LOOP ( 'NONE', ( #13053, #17280, #10056, #14941, #7334 ) ) ;
#5553 = FACE_OUTER_BOUND ( 'NONE', #9062, .T. ) ;
#5554 = CARTESIAN_POINT ( 'NONE',  ( 8.438534575730034959, 6.598402093327905504, -1.899950616255119407 ) ) ;
#5555 = CARTESIAN_POINT ( 'NONE',  ( 1.847340342630339860, 0.1245571717073309381, 12.44248139376886186 ) ) ;
#5556 = CARTESIAN_POINT ( 'NONE',  ( -30.00000000000000355, -12.50000000000000178, 6.000000000000000000 ) ) ;
#5557 = CYLINDRICAL_SURFACE ( 'NONE', #3880, 5.000000000000000888 ) ;
#5558 = ORIENTED_EDGE ( 'NONE', *, *, #9939, .F. ) ;
#5559 = CARTESIAN_POINT ( 'NONE',  ( 0.3142011359265348691, 10.88514493056454135, -8.382042760265784764 ) ) ;
#5560 = FILL_AREA_STYLE ('',( #2603 ) ) ;
#5561 = ADVANCED_BREP_SHAPE_REPRESENTATION ( '', ( #10500, #2030 ), #9034 ) ;
#5562 = ORIENTED_EDGE ( 'NONE', *, *, #16833, .F. ) ;
#5563 = EDGE_CURVE ( 'NONE', #12162, #8069, #3139, .T. ) ;
#5564 = VERTEX_POINT ( 'NONE', #7958 ) ;
#5565 = FACE_OUTER_BOUND ( 'NONE', #4907, .T. ) ;
#5566 = ORIENTED_EDGE ( 'NONE', *, *, #13261, .F. ) ;
#5567 = DIRECTION ( 'NONE',  ( 0.000000000000000000, 0.000000000000000000, 1.000000000000000000 ) ) ;
#5568 = VERTEX_POINT ( 'NONE', #17888 ) ;
#5569 = CIRCLE ( 'NONE', #8047, 4.750000000000000000 ) ;
#5570 = EDGE_CURVE ( 'NONE', #1472, #8587, #17607, .T. ) ;
#5571 = DIRECTION ( 'NONE',  ( 0.000000000000000000, 0.000000000000000000, 1.000000000000000000 ) ) ;
#5572 = CARTESIAN_POINT ( 'NONE',  ( 1.847461586945727152, -10.08650590720931284, -7.286856109515166047 ) ) ;
#5573 = CARTESIAN_POINT ( 'NONE',  ( 16.56872352241294521, -0.007512283835805501873, -0.007240717549633963156 ) ) ;
#5574 = CARTESIAN_POINT ( 'NONE',  ( 2.636624412715137922, -7.605649742761668719, 14.14563173255331741 ) ) ;
#5575 = DIRECTION ( 'NONE',  ( 1.000000000000000000, 0.000000000000000000, 0.000000000000000000 ) ) ;
#5576 = CARTESIAN_POINT ( 'NONE',  ( 16.56782317627811096, 0.009814734722107082768, 0.0003415813796006631126 ) ) ;
#5577 = B_SPLINE_CURVE_WITH_KNOTS ( 'NONE', 3,
 ( #4694, #10523, #16058, #4310 ),
 .UNSPECIFIED., .F., .F.,
 ( 4, 4 ),
 ( 2.359479019930958314E-17, 0.003005512676784853534 ),
 .UNSPECIFIED. ) ;
#5578 = FACE_OUTER_BOUND ( 'NONE', #17867, .T. ) ;
#5579 = CARTESIAN_POINT ( 'NONE',  ( 8.438534575730034959, 3.845978796786037268, 5.688336279099058146 ) ) ;
#5580 = VECTOR ( 'NONE', #10132, 1000.000000000000000 ) ;
#5581 = CIRCLE ( 'NONE', #1628, 14.54644660717763927 ) ;
#5582 = ORIENTED_EDGE ( 'NONE', *, *, #5547, .T. ) ;
#5583 = ORIENTED_EDGE ( 'NONE', *, *, #1004, .F. ) ;
#5584 = ORIENTED_EDGE ( 'NONE', *, *, #7779, .F. ) ;
#5585 = EDGE_LOOP ( 'NONE', ( #13903, #12683, #8675, #14963 ) ) ;
#5586 = ORIENTED_EDGE ( 'NONE', *, *, #1420, .F. ) ;
#5587 = EDGE_CURVE ( 'NONE', #13548, #11500, #18357, .T. ) ;
#5588 = CARTESIAN_POINT ( 'NONE',  ( 15.00000000000000711, -45.00000000000000000, 3.000000000000000000 ) ) ;
#5589 = CARTESIAN_POINT ( 'NONE',  ( 16.56872352241294521, 0.004564908236399969378, -0.009382111268607383134 ) ) ;
#5590 = CARTESIAN_POINT ( 'NONE',  ( 0.3145734862173252266, 8.321353293018990627, -10.93207848441423913 ) ) ;
#5591 = ORIENTED_EDGE ( 'NONE', *, *, #9626, .F. ) ;
#5592 = CARTESIAN_POINT ( 'NONE',  ( 2.353870697619112384, 12.92712089195302738, 0.7635393531606785578 ) ) ;
#5593 = DIRECTION ( 'NONE',  ( 1.000000000000000000, 0.000000000000000000, 0.000000000000000000 ) ) ;
#5594 = CIRCLE ( 'NONE', #14762, 14.54644660717763927 ) ;
#5595 = CIRCLE ( 'NONE', #3786, 14.54644660717763927 ) ;
#5596 = CARTESIAN_POINT ( 'NONE',  ( 5.045697689580606493, 7.500000000000000888, -13.04808138403512885 ) ) ;
#5597 = CARTESIAN_POINT ( 'NONE',  ( 0.3150692679895978898, -11.20465057551030874, 7.951395415075045214 ) ) ;
#5598 = LINE ( 'NONE', #11449, #9339 ) ;
#5599 = DIRECTION ( 'NONE',  ( 0.000000000000000000, 0.000000000000000000, -1.000000000000000000 ) ) ;
#5600 = CARTESIAN_POINT ( 'NONE',  ( -194.9999999999999716, -10.00000000000002665, 6.000000000000000000 ) ) ;
#5601 = CARTESIAN_POINT ( 'NONE',  ( 1.846138399168762989, -4.238866729160486457, 11.69739621335920710 ) ) ;
#5602 = VERTEX_POINT ( 'NONE', #7762 ) ;
#5603 = ORIENTED_EDGE ( 'NONE', *, *, #8436, .T. ) ;
#5604 = DIRECTION ( 'NONE',  ( -1.000000000000000000, -0.000000000000000000, -0.000000000000000000 ) ) ;
#5605 = CARTESIAN_POINT ( 'NONE',  ( 16.56753206892534891, -0.006760771273036220858, -0.006669401563384898778 ) ) ;
#5606 = VECTOR ( 'NONE', #18812, 1000.000000000000000 ) ;
#5607 = VERTEX_POINT ( 'NONE', #12426 ) ;
#5608 = DIRECTION ( 'NONE',  ( 0.000000000000000000, 1.000000000000000000, 0.000000000000000000 ) ) ;
#5609 = EDGE_CURVE ( 'NONE', #16284, #13343, #7650, .T. ) ;
#5610 = EDGE_CURVE ( 'NONE', #1583, #11395, #2286, .T. ) ;
#5611 = ORIENTED_EDGE ( 'NONE', *, *, #10206, .F. ) ;
#5612 = ADVANCED_FACE ( 'NONE', ( #18072 ), #18444, .F. ) ;
#5613 = CARTESIAN_POINT ( 'NONE',  ( 1.846138399168762101, -6.971848976710933954, -10.30487220521577818 ) ) ;
#5614 = DIRECTION ( 'NONE',  ( -0.000000000000000000, -0.000000000000000000, 1.000000000000000000 ) ) ;
#5615 = CARTESIAN_POINT ( 'NONE',  ( 16.56872352241294521, -0.004564908236400030961, 0.009382111268607351909 ) ) ;
#5616 = CARTESIAN_POINT ( 'NONE',  ( 1.845756295923359769, -11.97166802574123423, -3.386818134580184658 ) ) ;
#5617 = EDGE_LOOP ( 'NONE', ( #18004, #16089 ) ) ;
#5618 = PLANE ( 'NONE',  #10361 ) ;
#5619 = DIRECTION ( 'NONE',  ( -1.000000000000000000, -0.000000000000000000, -0.000000000000000000 ) ) ;
#5620 = DIRECTION ( 'NONE',  ( -0.000000000000000000, -0.5000000000000003331, -0.8660254037844384856 ) ) ;
#5621 = CIRCLE ( 'NONE', #16335, 0.2000000000000000944 ) ;
#5622 = DIRECTION ( 'NONE',  ( -1.000000000000000000, -0.000000000000000000, -0.000000000000000000 ) ) ;
#5623 = CARTESIAN_POINT ( 'NONE',  ( 3.353306896162455697, 1.348936822033017124, -13.88482890973694950 ) ) ;
#5624 = CONICAL_SURFACE ( 'NONE', #7497, 1732.050807568857181, 1.047197551196592746 ) ;
#5625 = VECTOR ( 'NONE', #5143, 1000.000000000000114 ) ;
#5626 = DIRECTION ( 'NONE',  ( 0.4460047087583925429, -0.8948208031649687033, -0.01937859614475526820 ) ) ;
#5627 = CARTESIAN_POINT ( 'NONE',  ( 3.686287386450715076E-15, -16.60000000000000142, 25.01316734529526187 ) ) ;
#5628 = CARTESIAN_POINT ( 'NONE',  ( 1.847168016377982669, 7.161712042621604546, -10.17509564929251020 ) ) ;
#5630 = ORIENTED_EDGE ( 'NONE', *, *, #6223, .F. ) ;
#5629 = CARTESIAN_POINT ( 'NONE',  ( 1.861628059977344263, 6.879051339207292948, 10.38573835516714716 ) ) ;
#5631 = CARTESIAN_POINT ( 'NONE',  ( 16.56679352167444819, -0.001518074900130714439, 0.009170718284672536857 ) ) ;
#5632 = CARTESIAN_POINT ( 'NONE',  ( 0.3151928476913548050, -13.06684726503523919, -4.245457024760359133 ) ) ;
#5633 = ORIENTED_EDGE ( 'NONE', *, *, #3300, .T. ) ;
#5634 = CARTESIAN_POINT ( 'NONE',  ( 1.846138399168762989, 10.30487220521570357, 6.971848976711047641 ) ) ;
#5635 = CARTESIAN_POINT ( 'NONE',  ( 2.002547531651519996, 12.57989064830759496, -0.6781519942172177240 ) ) ;
#5636 = CIRCLE ( 'NONE', #9017, 16.06066017081991149 ) ;
#5637 = ORIENTED_EDGE ( 'NONE', *, *, #9706, .F. ) ;
#5638 = CARTESIAN_POINT ( 'NONE',  ( 16.56753206892534891, -0.009369540855502522109, 0.001549402974394259360 ) ) ;
#5639 = FACE_OUTER_BOUND ( 'NONE', #6609, .T. ) ;
#5640 = ADVANCED_FACE ( 'NONE', ( #9373 ), #17005, .F. ) ;
#5641 = DIRECTION ( 'NONE',  ( 1.000000000000000000, 0.000000000000000000, 0.000000000000000000 ) ) ;
#5642 = CARTESIAN_POINT ( 'NONE',  ( 0.3137051932979792457, -11.37800749014136592, 7.698472063774431717 ) ) ;
#5643 = DIRECTION ( 'NONE',  ( -0.000000000000000000, -1.000000000000000000, -0.000000000000000000 ) ) ;
#5644 =( BOUNDED_SURFACE ( )  B_SPLINE_SURFACE ( 3, 1, ( 
 ( #3060, #13019 ),
 ( #7395, #2870 ),
 ( #3161, #10251 ),
 ( #5646, #10153 ) ),
 .UNSPECIFIED., .F., .F., .T. ) 
 B_SPLINE_SURFACE_WITH_KNOTS ( ( 4, 4 ),
 ( 2, 2 ),
 ( 0.000000000000000000, 1.000000000000000000 ),
 ( 0.000000000000000000, 1.000000000000000000 ),
 .UNSPECIFIED. ) 
 GEOMETRIC_REPRESENTATION_ITEM ( )  RATIONAL_B_SPLINE_SURFACE ( (
 ( 1.000000000000000000, 1.000000000000000000),
 ( 0.7792777138730158093, 0.9689936506012928330),
 ( 0.7792777138730158093, 0.9689936506012928330),
 ( 1.000000000000000000, 1.000000000000000000) ) ) 
 REPRESENTATION_ITEM ( '' )  SURFACE ( )  );
#5645 = CARTESIAN_POINT ( 'NONE',  ( 2.636624412715137478, -2.862162146983530775, 15.80357026013314048 ) ) ;
#5646 = CARTESIAN_POINT ( 'NONE',  ( 16.56872352241294521, -0.007240717549633941472, -0.007512283835804289302 ) ) ;
#5647 = CONICAL_SURFACE ( 'NONE', #12674, 2.100000000000000977, 1.029744258676656532 ) ;
#5648 = MECHANICAL_DESIGN_GEOMETRIC_PRESENTATION_REPRESENTATION (  '', ( #13907 ), #18786 ) ;
#5649 = CARTESIAN_POINT ( 'NONE',  ( 2.002547531651519996, -7.942910686618240845, 9.778737580845669797 ) ) ;
#5650 = CARTESIAN_POINT ( 'NONE',  ( 1.847412631396506244, 3.804043368582664009, 11.84727953344284579 ) ) ;
#5651 = CARTESIAN_POINT ( 'NONE',  ( 16.56782317627811096, -0.006045301465876687375, -0.007739510688078416953 ) ) ;
#5652 = EDGE_LOOP ( 'NONE', ( #2836, #954 ) ) ;
#5653 = CARTESIAN_POINT ( 'NONE',  ( 3.353306896162453477, -10.44017738170049903, -9.252610477110389198 ) ) ;
#5654 = CARTESIAN_POINT ( 'NONE',  ( 0.3095370825347233956, 8.444334731364008917, 10.84046130709061373 ) ) ;
#5655 = ORIENTED_EDGE ( 'NONE', *, *, #8895, .T. ) ;
#5656 = ORIENTED_EDGE ( 'NONE', *, *, #560, .T. ) ;
#5657 = CARTESIAN_POINT ( 'NONE',  ( 0.3170788640506441158, -7.952793437297652090, 11.20690911610900997 ) ) ;
#5658 = ORIENTED_EDGE ( 'NONE', *, *, #10179, .F. ) ;
#5659 = DIRECTION ( 'NONE',  ( 0.000000000000000000, 0.000000000000000000, 1.000000000000000000 ) ) ;
#5660 = ADVANCED_FACE ( 'NONE', ( #16457 ), #18256, .T. ) ;
#5661 = ORIENTED_EDGE ( 'NONE', *, *, #9078, .T. ) ;
#5662 = EDGE_CURVE ( 'NONE', #9516, #6835, #2201, .T. ) ;
#5663 = CIRCLE ( 'NONE', #12999, 1.000000000000000000 ) ;
#5664 = DIRECTION ( 'NONE',  ( 0.000000000000000000, 0.000000000000000000, 1.000000000000000000 ) ) ;
#5665 = CARTESIAN_POINT ( 'NONE',  ( 0.3150692679895968906, 13.11337225490258263, -4.099798979280710576 ) ) ;
#5666 = DIRECTION ( 'NONE',  ( 0.7635533937278216055, 0.6453904417649386493, 0.02138673900302558509 ) ) ;
#5667 = CARTESIAN_POINT ( 'NONE',  ( 1.254009781012375813, 11.25324419414251942, -9.426200207652035701 ) ) ;
#5668 = CARTESIAN_POINT ( 'NONE',  ( 0.3137051932979775248, -12.91601973349273891, 4.679953077377436266 ) ) ;
#5669 = CARTESIAN_POINT ( 'NONE',  ( -61.35602477868047799, -15.00000000000001066, 3.000000000000002665 ) ) ;
#5670 = CARTESIAN_POINT ( 'NONE',  ( 16.56679352167444819, -0.006526964904752395082, 0.006618561353600064395 ) ) ;
#5671 = CARTESIAN_POINT ( 'NONE',  ( 2.636624412715137034, -11.60464335004055947, 11.10302021257951743 ) ) ;
#5672 = EDGE_CURVE ( 'NONE', #12599, #8470, #1256, .T. ) ;
#5673 = VECTOR ( 'NONE', #15431, 1000.000000000000000 ) ;
#5674 = ORIENTED_EDGE ( 'NONE', *, *, #12977, .T. ) ;
#5675 = AXIS2_PLACEMENT_3D ( 'NONE', #7181, #6192, #5721 ) ;
#5676 = ORIENTED_EDGE ( 'NONE', *, *, #3834, .T. ) ;
#5677 = AXIS2_PLACEMENT_3D ( 'NONE', #16675, #8173, #13986 ) ;
#5678 = VERTEX_POINT ( 'NONE', #15290 ) ;
#5679 = ORIENTED_EDGE ( 'NONE', *, *, #7639, .T. ) ;
#5680 =( BOUNDED_SURFACE ( )  B_SPLINE_SURFACE ( 3, 1, ( 
 ( #14458, #10161 ),
 ( #13408, #14940 ),
 ( #4334, #324 ),
 ( #17426, #10449 ) ),
 .UNSPECIFIED., .F., .F., .T. ) 
 B_SPLINE_SURFACE_WITH_KNOTS ( ( 4, 4 ),
 ( 2, 2 ),
 ( 0.000000000000000000, 1.000000000000000000 ),
 ( 0.000000000000000000, 1.000000000000000000 ),
 .UNSPECIFIED. ) 
 GEOMETRIC_REPRESENTATION_ITEM ( )  RATIONAL_B_SPLINE_SURFACE ( (
 ( 1.000000000000000000, 1.000000000000000000),
 ( 0.9593108457356467333, 0.9995965569486454649),
 ( 0.9593108457356467333, 0.9995965569486454649),
 ( 1.000000000000000000, 1.000000000000000000) ) ) 
 REPRESENTATION_ITEM ( '' )  SURFACE ( )  );
#5681 = ORIENTED_EDGE ( 'NONE', *, *, #11569, .T. ) ;
#5682 = CARTESIAN_POINT ( 'NONE',  ( 4.000000000000000888, 17.00000000000000000, 7.000000000000000000 ) ) ;
#5683 = CIRCLE ( 'NONE', #15470, 5.000000000000000000 ) ;
#5684 = APPLICATION_CONTEXT ( 'automotive_design' ) ;
#5685 = CARTESIAN_POINT ( 'NONE',  ( 2.636624412716062515, -6.973567714909003179, -14.46769361191335790 ) ) ;
#5686 = CARTESIAN_POINT ( 'NONE',  ( 16.56822296793089322, -0.01011126603341077138, 0.0007467251401298242519 ) ) ;
#5687 = VERTEX_POINT ( 'NONE', #5515 ) ;
#5688 = CARTESIAN_POINT ( 'NONE',  ( 15.00000000000000711, -39.99999999999999289, 3.000000000000000000 ) ) ;
#5689 = CIRCLE ( 'NONE', #16409, 13.42403576283810906 ) ;
#5690 = DIRECTION ( 'NONE',  ( -1.000000000000000000, -0.000000000000000000, -0.000000000000000000 ) ) ;
#5691 = CARTESIAN_POINT ( 'NONE',  ( 0.5544330523544508393, 7.499999999999999112, -14.29923508549706135 ) ) ;
#5692 = DIRECTION ( 'NONE',  ( -1.540743955509788340E-33, -1.000000000000000000, -2.533398541561209262E-17 ) ) ;
#5693 = CARTESIAN_POINT ( 'NONE',  ( 0.3058872367615226295, 3.664492643742762290, 13.24582953854926615 ) ) ;
#5694 = CARTESIAN_POINT ( 'NONE',  ( 0.4754618798421171855, -13.89949764182683190, 0.7484603771383911974 ) ) ;
#5695 = DIRECTION ( 'NONE',  ( -1.000000000000000000, -0.000000000000000000, -0.000000000000000000 ) ) ;
#5696 = DIRECTION ( 'NONE',  ( 1.000000000000000000, 0.000000000000000000, 0.000000000000000000 ) ) ;
#5697 = B_SPLINE_CURVE_WITH_KNOTS ( 'NONE', 3,
 ( #9640, #13942, #14930, #1847, #12596, #16376, #13401, #7687, #3262, #15025, #3720, #14040, #8040 ),
 .UNSPECIFIED., .F., .F.,
 ( 4, 3, 3, 3, 4 ),
 ( 3.878959614448864246E-18, 0.0002299780670421069050, 0.0004599561239687931019, 0.0006896788984287867625, 0.0009194956271626391958 ),
 .UNSPECIFIED. ) ;
#5698 = CARTESIAN_POINT ( 'NONE',  ( 1.846955891736115962, -3.593597880662430910, 11.91257079808167596 ) ) ;
#5699 = EDGE_CURVE ( 'NONE', #11329, #12087, #13643, .T. ) ;
#5700 = ORIENTED_EDGE ( 'NONE', *, *, #4312, .F. ) ;
#5701 = VERTEX_POINT ( 'NONE', #3816 ) ;
#5702 = VERTEX_POINT ( 'NONE', #2996 ) ;
#5703 = ORIENTED_EDGE ( 'NONE', *, *, #14176, .T. ) ;
#5704 = CARTESIAN_POINT ( 'NONE',  ( 3.074695600507272086, 14.01296402267896291, -6.754521329824639153 ) ) ;
#5705 = VERTEX_POINT ( 'NONE', #17546 ) ;
#5706 = CARTESIAN_POINT ( 'NONE',  ( -194.9999999999999716, -10.00000000000002665, 3.000000000000000000 ) ) ;
#5707 = CARTESIAN_POINT ( 'NONE',  ( 2.002547531651519996, 6.845637710436190737, 10.57595306287294612 ) ) ;
#5708 = CARTESIAN_POINT ( 'NONE',  ( 3.074695600507137083, -11.23985886659436773, -10.75417554975720869 ) ) ;
#5709 = B_SPLINE_CURVE_WITH_KNOTS ( 'NONE', 3,
 ( #4912, #12178, #13702, #9490, #16573, #3466 ),
 .UNSPECIFIED., .F., .F.,
 ( 4, 2, 4 ),
 ( 0.000000000000000000, 0.001656992708822040920, 0.003313985417644081839 ),
 .UNSPECIFIED. ) ;
#5710 = CARTESIAN_POINT ( 'NONE',  ( 0.3170788640506440603, -4.100430649997872656, -13.11595226728161911 ) ) ;
#5711 = ORIENTED_EDGE ( 'NONE', *, *, #14301, .F. ) ;
#5712 = CARTESIAN_POINT ( 'NONE',  ( 16.57778382496167424, -0.01306626476309383916, -0.007244066302947642193 ) ) ;
#5713 = VECTOR ( 'NONE', #6370, 1000.000000000000227 ) ;
#5714 = CARTESIAN_POINT ( 'NONE',  ( 1.845755665166726844, 3.386720041070728104, 11.97169564665392727 ) ) ;
#5715 = CARTESIAN_POINT ( 'NONE',  ( 0.3142014840576499712, -13.73311050063163563, -0.3830336514510319090 ) ) ;
#5716 = CARTESIAN_POINT ( 'NONE',  ( 0.000000000000000000, 0.000000000000000000, 0.000000000000000000 ) ) ;
#5717 = B_SPLINE_CURVE_WITH_KNOTS ( 'NONE', 3,
 ( #14082, #9960, #12552, #18566, #6823, #11043 ),
 .UNSPECIFIED., .F., .F.,
 ( 4, 2, 4 ),
 ( 0.000000000000000000, 0.0001828790815886955387, 0.0003657581631773888006 ),
 .UNSPECIFIED. ) ;
#5718 = CARTESIAN_POINT ( 'NONE',  ( 3.950837973638675393, -10.51028938476224894, 10.05648675950122595 ) ) ;
#5719 = CARTESIAN_POINT ( 'NONE',  ( 0.4862570985993235340, -12.97920246947883172, 5.003653737315437944 ) ) ;
#5720 = ADVANCED_FACE ( 'NONE', ( #946 ), #873, .F. ) ;
#5721 = DIRECTION ( 'NONE',  ( 1.000000000000000000, 0.000000000000000000, 0.000000000000000000 ) ) ;
#5722 = FACE_OUTER_BOUND ( 'NONE', #5208, .T. ) ;
#5723 = EDGE_CURVE ( 'NONE', #10455, #8123, #5390, .T. ) ;
#5724 = ADVANCED_FACE ( 'NONE', ( #8495 ), #14322, .T. ) ;
#5725 = ORIENTED_EDGE ( 'NONE', *, *, #489, .F. ) ;
#5726 = CARTESIAN_POINT ( 'NONE',  ( 4.755015822784811164, -4.336808689942017736E-16, 0.000000000000000000 ) ) ;
#5728 = EDGE_LOOP ( 'NONE', ( #9335, #18744, #5876, #12627 ) ) ;
#5727 = CARTESIAN_POINT ( 'NONE',  ( 0.3137051932979792457, 13.20008686438105983, 3.805684345189833451 ) ) ;
#5729 = DIRECTION ( 'NONE',  ( 0.000000000000000000, 0.000000000000000000, 1.000000000000000000 ) ) ;
#5730 = CARTESIAN_POINT ( 'NONE',  ( 0.3145729642390373559, -13.15786090015081555, -3.952965287571249764 ) ) ;
#5731 = ORIENTED_EDGE ( 'NONE', *, *, #14910, .F. ) ;
#5732 = CARTESIAN_POINT ( 'NONE',  ( 1.847461586945732037, 10.08650590720936258, 7.286856109515091440 ) ) ;
#5733 = DIRECTION ( 'NONE',  ( -1.000000000000000000, 0.000000000000000000, 0.000000000000000000 ) ) ;
#5734 = ADVANCED_FACE ( 'NONE', ( #3912 ), #15471, .F. ) ;
#5735 = EDGE_LOOP ( 'NONE', ( #12939, #14826, #4462, #12444 ) ) ;
#5736 = CARTESIAN_POINT ( 'NONE',  ( 16.56753206892534891, -0.001549402974394225099, -0.009369540855502527313 ) ) ;
#5737 = CARTESIAN_POINT ( 'NONE',  ( 0.3142014840576534684, -4.608051180497015231, 12.94260032291127160 ) ) ;
#5738 = CARTESIAN_POINT ( 'NONE',  ( 0.3148208552358952028, -10.97826876274317875, 8.260375059853302560 ) ) ;
#5739 = ORIENTED_EDGE ( 'NONE', *, *, #18650, .T. ) ;
#5740 =( NAMED_UNIT ( * ) PLANE_ANGLE_UNIT ( ) SI_UNIT ( $, .RADIAN. ) );
#5741 = CARTESIAN_POINT ( 'NONE',  ( 1.560000000000000053, 0.000000000000000000, 2.999999999999998668 ) ) ;
#5742 = DIRECTION ( 'NONE',  ( 0.000000000000000000, 1.000000000000000000, 0.000000000000000000 ) ) ;
#5743 = CARTESIAN_POINT ( 'NONE',  ( 2.002547531651519996, 11.75462648437108015, -4.532360870844206246 ) ) ;
#5744 = CYLINDRICAL_SURFACE ( 'NONE', #9288, 4.999999999999997335 ) ;
#5745 = CARTESIAN_POINT ( 'NONE',  ( 2.002547531651519996, -12.57989064830759141, -0.6781519942173057647 ) ) ;
#5746 = EDGE_CURVE ( 'NONE', #3723, #14463, #4482, .T. ) ;
#5747 = EDGE_CURVE ( 'NONE', #17499, #1936, #3566, .T. ) ;
#5748 = ORIENTED_EDGE ( 'NONE', *, *, #15596, .T. ) ;
#5749 = CARTESIAN_POINT ( 'NONE',  ( 2.320521194582820801, -15.43440938317095146, -3.126729093671786863 ) ) ;
#5750 = LINE ( 'NONE', #13124, #10278 ) ;
#5751 = B_SPLINE_CURVE_WITH_KNOTS ( 'NONE', 3,
 ( #4566, #6096, #13447, #4369 ),
 .UNSPECIFIED., .F., .F.,
 ( 4, 4 ),
 ( 0.000000000000000000, 0.002004993803842607548 ),
 .UNSPECIFIED. ) ;
#5752 = EDGE_LOOP ( 'NONE', ( #10118, #4271, #15821 ) ) ;
#5753 = VERTEX_POINT ( 'NONE', #14042 ) ;
#5754 = LINE ( 'NONE', #14071, #8494 ) ;
#5755 = ORIENTED_EDGE ( 'NONE', *, *, #13094, .T. ) ;
#5756 = DIRECTION ( 'NONE',  ( -0.000000000000000000, -0.5000000000000003331, -0.8660254037844384856 ) ) ;
#5757 = VECTOR ( 'NONE', #8899, 1000.000000000000114 ) ;
#5758 = B_SPLINE_CURVE_WITH_KNOTS ( 'NONE', 3,
 ( #11011, #2211, #13958, #12435, #779, #2559, #15570, #9476, #12707, #17023, #5257, #2472, #15391 ),
 .UNSPECIFIED., .F., .F.,
 ( 4, 3, 3, 3, 4 ),
 ( 3.127317220692750759E-18, 0.0002299804304191498290, 0.0004599608082120264186, 0.0006467586077648000654, 0.0008336169836825974228 ),
 .UNSPECIFIED. ) ;
#5759 = VECTOR ( 'NONE', #14419, 1000.000000000000000 ) ;
#5760 = ORIENTED_EDGE ( 'NONE', *, *, #12471, .T. ) ;
#5761 = ADVANCED_FACE ( 'NONE', ( #1031 ), #11146, .F. ) ;
#5762 = CARTESIAN_POINT ( 'NONE',  ( 1.560000000000000053, 1.732050807568878747, 7.017607234860990640E-28 ) ) ;
#5763 =( BOUNDED_SURFACE ( )  B_SPLINE_SURFACE ( 3, 1, ( 
 ( #3885, #18776 ),
 ( #16977, #14382 ),
 ( #9887, #9712 ),
 ( #18495, #15719 ) ),
 .UNSPECIFIED., .F., .F., .T. ) 
 B_SPLINE_SURFACE_WITH_KNOTS ( ( 4, 4 ),
 ( 2, 2 ),
 ( 0.000000000000000000, 1.000000000000000000 ),
 ( 0.000000000000000000, 1.000000000000000000 ),
 .UNSPECIFIED. ) 
 GEOMETRIC_REPRESENTATION_ITEM ( )  RATIONAL_B_SPLINE_SURFACE ( (
 ( 1.000000000000000000, 1.000000000000000000),
 ( 0.7792777138730160313, 0.9689936506012927220),
 ( 0.7792777138730160313, 0.9689936506012927220),
 ( 1.000000000000000000, 1.000000000000000000) ) ) 
 REPRESENTATION_ITEM ( '' )  SURFACE ( )  );
#5764 = CARTESIAN_POINT ( 'NONE',  ( 0.3095370825347234511, -10.84046130709052314, -8.444334731364126156 ) ) ;
#5765 = AXIS2_PLACEMENT_3D ( 'NONE', #11077, #3525, #15455 ) ;
#5766 = DIRECTION ( 'NONE',  ( 1.000000000000000000, 0.000000000000000000, 0.000000000000000000 ) ) ;
#5767 = CARTESIAN_POINT ( 'NONE',  ( 0.3170788640506441158, -0.1533108587035203196, -13.74111462631963576 ) ) ;
#5768 = LINE ( 'NONE', #8746, #11390 ) ;
#5769 = CARTESIAN_POINT ( 'NONE',  ( 1.861706995891667882, 4.359009869687244354, 11.66987142852985748 ) ) ;
#5770 = AXIS2_PLACEMENT_3D ( 'NONE', #5523, #14329, #18710 ) ;
#5771 = CARTESIAN_POINT ( 'NONE',  ( 2.123976203522053741, 13.47898556379313284, 7.899625852120258251 ) ) ;
#5772 = CARTESIAN_POINT ( 'NONE',  ( 3.074695600507258320, -7.366518011946037170, 13.70113613813197873 ) ) ;
#5773 = ORIENTED_EDGE ( 'NONE', *, *, #14557, .F. ) ;
#5774 = EDGE_CURVE ( 'NONE', #13838, #13455, #5093, .T. ) ;
#5775 = VERTEX_POINT ( 'NONE', #15646 ) ;
#5776 = ORIENTED_EDGE ( 'NONE', *, *, #13131, .F. ) ;
#5777 = ORIENTED_EDGE ( 'NONE', *, *, #4214, .T. ) ;
#5778 = EDGE_LOOP ( 'NONE', ( #2508, #2646, #841, #2040, #1250 ) ) ;
#5779 = ADVANCED_FACE ( 'NONE', ( #2549 ), #10280, .T. ) ;
#5780 = LINE ( 'NONE', #4272, #3143 ) ;
#5781 = B_SPLINE_CURVE_WITH_KNOTS ( 'NONE', 3,
 ( #15033, #16182, #4720, #4530 ),
 .UNSPECIFIED., .F., .F.,
 ( 4, 4 ),
 ( 1.927807806696441531E-17, 0.003005512676784856570 ),
 .UNSPECIFIED. ) ;
#5782 = CARTESIAN_POINT ( 'NONE',  ( 0.8740779401510756497, -5.211551231203870316, -13.31469722824378721 ) ) ;
#5783 = CARTESIAN_POINT ( 'NONE',  ( 16.56872352241294521, -0.01027347319884440620, 0.001821578298044753286 ) ) ;
#5784 = VERTEX_POINT ( 'NONE', #8312 ) ;
#5785 = DIRECTION ( 'NONE',  ( -1.000000000000000000, -0.000000000000000000, -0.000000000000000000 ) ) ;
#5786 = EDGE_CURVE ( 'NONE', #16287, #13879, #14861, .T. ) ;
#5787 = CARTESIAN_POINT ( 'NONE',  ( 2.636624412714236865, 0.000000000000000000, 0.000000000000000000 ) ) ;
#5788 = DIRECTION ( 'NONE',  ( -0.000000000000000000, -0.000000000000000000, 1.000000000000000000 ) ) ;
#5789 = CARTESIAN_POINT ( 'NONE',  ( 2.123976203522053297, -3.347755036805797779, -15.26039569100262838 ) ) ;
#5790 = CARTESIAN_POINT ( 'NONE',  ( 0.3151926232592536792, -11.07013665200800645, 8.137833541809341042 ) ) ;
#5791 = SPHERICAL_SURFACE ( 'NONE', #12083, 5.000000000000000000 ) ;
#5792 = CARTESIAN_POINT ( 'NONE',  ( 2.002547531651521773, 9.778737580845699995, 7.942910686618207983 ) ) ;
#5793 = B_SPLINE_CURVE_WITH_KNOTS ( 'NONE', 3,
 ( #12543, #11126, #889, #13983, #5190, #11226 ),
 .UNSPECIFIED., .F., .F.,
 ( 4, 2, 4 ),
 ( 3.556447555475521540E-17, 0.0001825746017570583171, 0.0003651492035140810723 ),
 .UNSPECIFIED. ) ;
#5794 = DIRECTION ( 'NONE',  ( -0.000000000000000000, 1.000000000000000000, -0.000000000000000000 ) ) ;
#5795 = CARTESIAN_POINT ( 'NONE',  ( 2.697797270744668463, 4.970631985779762729, -12.33058466479263693 ) ) ;
#5796 = EDGE_LOOP ( 'NONE', ( #10652, #18073, #16821, #7183 ) ) ;
#5797 = SHAPE_REPRESENTATION ( 'Handle arm 2', ( #2030 ), #14825 ) ;
#5798 =( BOUNDED_SURFACE ( )  B_SPLINE_SURFACE ( 3, 1, ( 
 ( #16723, #3801 ),
 ( #3623, #18329 ),
 ( #9632, #15458 ),
 ( #14032, #1303 ) ),
 .UNSPECIFIED., .F., .F., .T. ) 
 B_SPLINE_SURFACE_WITH_KNOTS ( ( 4, 4 ),
 ( 2, 2 ),
 ( 0.000000000000000000, 1.000000000000000000 ),
 ( 0.000000000000000000, 1.000000000000000000 ),
 .UNSPECIFIED. ) 
 GEOMETRIC_REPRESENTATION_ITEM ( )  RATIONAL_B_SPLINE_SURFACE ( (
 ( 1.000000000000000000, 1.000000000000000000),
 ( 0.9933953342250438912, 0.8357391271907739227),
 ( 0.9933953342250438912, 0.8357391271907739227),
 ( 1.000000000000000000, 1.000000000000000000) ) ) 
 REPRESENTATION_ITEM ( '' )  SURFACE ( )  );
#5799 = ORIENTED_EDGE ( 'NONE', *, *, #3967, .T. ) ;
#5800 = EDGE_LOOP ( 'NONE', ( #55, #6322, #16487, #14350, #16599, #4493, #16807, #13765, #8584, #4939, #6418, #15314, #6813, #550, #17398, #17307, #10144, #11, #640, #13943, #11433, #1830, #974, #14831, #8276, #16595, #17748, #16896, #1032, #18255, #5236, #14323, #16755, #10836, #15825, #2424, #14434, #6469, #2808, #10697, #1560, #12472, #2696, #10190, #6107, #8420, #16818, #9654, #17238, #17032, #1373, #157, #8673, #2874, #14285, #10724, #10263, #816, #15308, #10311, #8803, #9600, #2899, #1278 ) ) ;
#5801 = VERTEX_POINT ( 'NONE', #1131 ) ;
#5802 = FACE_OUTER_BOUND ( 'NONE', #1879, .T. ) ;
#5803 = ADVANCED_FACE ( 'NONE', ( #6977 ), #4092, .F. ) ;
#5804 = EDGE_LOOP ( 'NONE', ( #910, #13167, #15336, #6277 ) ) ;
#5805 = CARTESIAN_POINT ( 'NONE',  ( 3.074695600507694859, 14.01296402267844066, 6.754521329824622278 ) ) ;
#5806 = CARTESIAN_POINT ( 'NONE',  ( 3.353306896162453477, -9.252610477110343012, 10.44017738170053278 ) ) ;
#5807 = CARTESIAN_POINT ( 'NONE',  ( 8.438534575730034959, 5.688336279099100778, -3.845978796785973763 ) ) ;
#5808 = CARTESIAN_POINT ( 'NONE',  ( 16.56753206892534891, 0.006760771273036169683, 0.006669401563384943880 ) ) ;
#5809 = ORIENTED_EDGE ( 'NONE', *, *, #12320, .F. ) ;
#5810 = CARTESIAN_POINT ( 'NONE',  ( 1.845755665166725290, 0.4784952423730285953, -12.43231320373360660 ) ) ;
#5811 = EDGE_CURVE ( 'NONE', #14913, #8937, #9227, .T. ) ;
#5812 = CARTESIAN_POINT ( 'NONE',  ( 1.861628059977344263, 3.332996951203627933, 12.00316790821102941 ) ) ;
#5813 = DIRECTION ( 'NONE',  ( 0.000000000000000000, -1.000000000000000000, 0.000000000000000000 ) ) ;
#5814 = CARTESIAN_POINT ( 'NONE',  ( 0.3170788640506441158, 8.200855617524535290, 11.02668139258444846 ) ) ;
#5815 = CARTESIAN_POINT ( 'NONE',  ( 1.847247051441591070, 11.78111530882023317, 4.004229874809065670 ) ) ;
#5816 = FACE_BOUND ( 'NONE', #5352, .T. ) ;
#5817 = CARTESIAN_POINT ( 'NONE',  ( 20.00000000000000711, -19.99999999999999645, 3.000000000000000000 ) ) ;
#5818 = VERTEX_POINT ( 'NONE', #15157 ) ;
#5819 = VERTEX_POINT ( 'NONE', #4645 ) ;
#5820 = AXIS2_PLACEMENT_3D ( 'NONE', #15005, #7668, #11955 ) ;
#5821 = FACE_OUTER_BOUND ( 'NONE', #16597, .T. ) ;
#5823 = ORIENTED_EDGE ( 'NONE', *, *, #9025, .T. ) ;
#5822 = DIRECTION ( 'NONE',  ( -0.000000000000000000, -0.000000000000000000, 1.000000000000000000 ) ) ;
#5824 = CARTESIAN_POINT ( 'NONE',  ( 3.950837973638676281, -6.316429227969562632, 13.10350451991838128 ) ) ;
#5825 = CARTESIAN_POINT ( 'NONE',  ( 0.4862570985993252548, -5.003653737315580052, 12.97920246947877665 ) ) ;
#5826 = EDGE_LOOP ( 'NONE', ( #17522, #6906, #16386, #5522 ) ) ;
#5827 = CARTESIAN_POINT ( 'NONE',  ( 3.512766787570708260, -14.91422000116825508, -2.025881399556554552 ) ) ;
#5828 = B_SPLINE_CURVE_WITH_KNOTS ( 'NONE', 3,
 ( #13713, #629, #9412, #2151 ),
 .UNSPECIFIED., .F., .F.,
 ( 4, 4 ),
 ( 4.589925559575316169E-16, 0.002004993803842821786 ),
 .UNSPECIFIED. ) ;
#5829 = PRODUCT_DEFINITION_SHAPE ( 'NONE', 'NONE',  #9645 ) ;
#5830 = CARTESIAN_POINT ( 'NONE',  ( 6.118503526523853431, -3.404981712889560974, -11.99999999938682294 ) ) ;
#5831 = ORIENTED_EDGE ( 'NONE', *, *, #5857, .T. ) ;
#5832 = DIRECTION ( 'NONE',  ( 0.000000000000000000, 0.5000000000000003331, 0.8660254037844383745 ) ) ;
#5833 = EDGE_CURVE ( 'NONE', #15093, #8524, #11813, .T. ) ;
#5834 = EDGE_CURVE ( 'NONE', #14724, #13901, #12201, .T. ) ;
#5835 = ADVANCED_FACE ( 'NONE', ( #15054 ), #10287, .T. ) ;
#5836 = CARTESIAN_POINT ( 'NONE',  ( -2.500000000000000000, 3.061616997868383141E-16, -13.00000000000000533 ) ) ;
#5837 = DIRECTION ( 'NONE',  ( 0.7561779333270775005, -0.5491072561318390832, 0.3559159372837255031 ) ) ;
#5838 = FACE_OUTER_BOUND ( 'NONE', #5585, .T. ) ;
#5839 = CIRCLE ( 'NONE', #15930, 5.000000000000000000 ) ;
#5840 = PLANE ( 'NONE',  #17495 ) ;
#5841 = CARTESIAN_POINT ( 'NONE',  ( 0.3132635586635977853, 10.79541209008116454, -8.495712071659280440 ) ) ;
#5842 = CARTESIAN_POINT ( 'NONE',  ( 3.377929128793398572, 12.84367544717943410, -5.536064832134035996 ) ) ;
#5843 = CARTESIAN_POINT ( 'NONE',  ( 16.56753206892534891, 0.008490833999798002782, -0.004253784598196794220 ) ) ;
#5844 = PLANE ( 'NONE',  #15783 ) ;
#5845 = ORIENTED_EDGE ( 'NONE', *, *, #7440, .F. ) ;
#5846 = PLANE ( 'NONE',  #15780 ) ;
#5847 = CARTESIAN_POINT ( 'NONE',  ( 0.3095370825347224519, -12.91933430393611282, 4.681152801286110332 ) ) ;
#5848 = VERTEX_POINT ( 'NONE', #12005 ) ;
#5849 = ORIENTED_EDGE ( 'NONE', *, *, #8215, .F. ) ;
#5850 = CARTESIAN_POINT ( 'NONE',  ( 0.3137051932979757485, -4.679953077377398074, -12.91601973349275134 ) ) ;
#5851 = VERTEX_POINT ( 'NONE', #1972 ) ;
#5852 = DIRECTION ( 'NONE',  ( -1.000000000000000000, 0.000000000000000000, 0.000000000000000000 ) ) ;
#5853 = AXIS2_PLACEMENT_3D ( 'NONE', #10071, #2268, #6584 ) ;
#5854 = VERTEX_POINT ( 'NONE', #6273 ) ;
#5855 = EDGE_CURVE ( 'NONE', #6897, #15883, #10864, .T. ) ;
#5856 = ADVANCED_FACE ( 'NONE', ( #17838 ), #11982, .F. ) ;
#5857 = EDGE_CURVE ( 'NONE', #14019, #9425, #357, .T. ) ;
#5858 = CARTESIAN_POINT ( 'NONE',  ( 3.512766787570836158, 7.127386085302768848, 13.25664064834467837 ) ) ;
#5859 = CARTESIAN_POINT ( 'NONE',  ( 2.123976203522053741, 10.37815841598491851, 11.67822624909929452 ) ) ;
#5860 = DIRECTION ( 'NONE',  ( 0.7635533937278216055, 0.5095610256143827677, 0.3966532189476653092 ) ) ;
#5861 = EDGE_CURVE ( 'NONE', #13196, #17057, #443, .T. ) ;
#5862 = CARTESIAN_POINT ( 'NONE',  ( 1.846138399168762989, -4.238866729160486457, 11.69739621335920710 ) ) ;
#5863 = PLANE ( 'NONE',  #3815 ) ;
#5864 = DIRECTION ( 'NONE',  ( 0.7561779333270775005, -0.6106991889125055195, -0.2350349629540206264 ) ) ;
#5865 = SURFACE_STYLE_FILL_AREA ( #7616 ) ;
#5866 = CARTESIAN_POINT ( 'NONE',  ( 1.846613052777650976, 0.3401093050881815461, 12.43780859207239864 ) ) ;
#5867 = DIRECTION ( 'NONE',  ( -0.000000000000000000, -0.5000000000000004441, 0.8660254037844383745 ) ) ;
#5868 = LINE ( 'NONE', #11809, #13541 ) ;
#5869 = CARTESIAN_POINT ( 'NONE',  ( 0.3148208552358917611, 13.73693263646118723, -0.2299193288887949882 ) ) ;
#5870 = EDGE_LOOP ( 'NONE', ( #15390, #7937 ) ) ;
#5871 = CARTESIAN_POINT ( 'NONE',  ( 3.686287386450715076E-15, -16.60000000000000142, 25.01316734529526187 ) ) ;
#5872 = ORIENTED_EDGE ( 'NONE', *, *, #13033, .F. ) ;
#5873 = CIRCLE ( 'NONE', #14732, 2.100000000000000977 ) ;
#5874 = ORIENTED_EDGE ( 'NONE', *, *, #15813, .T. ) ;
#5875 = ORIENTED_EDGE ( 'NONE', *, *, #1048, .F. ) ;
#5876 = ORIENTED_EDGE ( 'NONE', *, *, #15813, .F. ) ;
#5877 =( BOUNDED_SURFACE ( )  B_SPLINE_SURFACE ( 3, 1, ( 
 ( #12925, #8356 ),
 ( #4145, #11412 ),
 ( #14173, #5388 ),
 ( #6922, #17051 ) ),
 .UNSPECIFIED., .F., .F., .T. ) 
 B_SPLINE_SURFACE_WITH_KNOTS ( ( 4, 4 ),
 ( 2, 2 ),
 ( 0.000000000000000000, 1.000000000000000000 ),
 ( 0.000000000000000000, 1.000000000000000000 ),
 .UNSPECIFIED. ) 
 GEOMETRIC_REPRESENTATION_ITEM ( )  RATIONAL_B_SPLINE_SURFACE ( (
 ( 1.000000000000000000, 1.000000000000000000),
 ( 0.9593108457356467333, 0.9995965569486454649),
 ( 0.9593108457356467333, 0.9995965569486454649),
 ( 1.000000000000000000, 1.000000000000000000) ) ) 
 REPRESENTATION_ITEM ( '' )  SURFACE ( )  );
#5878 = DIRECTION ( 'NONE',  ( -1.000000000000000000, 0.000000000000000000, 0.000000000000000000 ) ) ;
#5879 = CARTESIAN_POINT ( 'NONE',  ( 1.560000000000000053, 0.8660254037844389297, -1.500000000000000000 ) ) ;
#5880 = CARTESIAN_POINT ( 'NONE',  ( 0.3095370825347234511, 10.84046130709058708, 8.444334731364046220 ) ) ;
#5881 = ORIENTED_EDGE ( 'NONE', *, *, #7591, .F. ) ;
#5882 = CARTESIAN_POINT ( 'NONE',  ( 0.3058872367615226295, -7.578326039752520060, -11.46514199369366516 ) ) ;
#5883 = ADVANCED_FACE ( 'NONE', ( #3390 ), #6078, .F. ) ;
#5884 = CARTESIAN_POINT ( 'NONE',  ( 0.3132635586635976188, 0.5277914263193109745, 13.72732610560088773 ) ) ;
#5885 = EDGE_CURVE ( 'NONE', #13788, #3395, #9695, .T. ) ;
#5886 = DIRECTION ( 'NONE',  ( -1.000000000000000000, 0.000000000000000000, 0.000000000000000000 ) ) ;
#5887 = CARTESIAN_POINT ( 'NONE',  ( 5.000000000000000888, 17.00000000000000000, 8.000000000000000000 ) ) ;
#5888 = CARTESIAN_POINT ( 'NONE',  ( 0.3720661004400037664, 3.575426119359183197, 13.34435358167253938 ) ) ;
#5889 = VECTOR ( 'NONE', #9131, 1000.000000000000114 ) ;
#5890 = CYLINDRICAL_SURFACE ( 'NONE', #17248, 4.000000000000000000 ) ;
#5891 = CARTESIAN_POINT ( 'NONE',  ( 5.000000000000000000, 20.00000000000000000, 8.000000000000000000 ) ) ;
#5892 = CARTESIAN_POINT ( 'NONE',  ( 0.3151928479966097374, 1.775918418904422640E-15, 13.73922861026898623 ) ) ;
#5893 = CARTESIAN_POINT ( 'NONE',  ( 1.847034903785822690, 7.126331315909270714, 10.19974412751566994 ) ) ;
#5894 = EDGE_LOOP ( 'NONE', ( #314, #13600, #6404, #15748 ) ) ;
#5895 = ORIENTED_EDGE ( 'NONE', *, *, #12049, .T. ) ;
#5896 = VERTEX_POINT ( 'NONE', #15430 ) ;
#5897 = EDGE_CURVE ( 'NONE', #12510, #6753, #6288, .T. ) ;
#5898 = VERTEX_POINT ( 'NONE', #5115 ) ;
#5899 = CARTESIAN_POINT ( 'NONE',  ( 16.57778382496167424, 0.01466529584256784369, 0.002851818597094051173 ) ) ;
#5900 = CONICAL_SURFACE ( 'NONE', #6832, 16.06066017081991149, 0.7853981625000062694 ) ;
#5901 = ORIENTED_EDGE ( 'NONE', *, *, #10540, .T. ) ;
#5902 = CARTESIAN_POINT ( 'NONE',  ( 0.4754618798421162973, -11.68486377711971969, 7.564402563418428649 ) ) ;
#5903 = CIRCLE ( 'NONE', #16610, 16.06066017081991149 ) ;
#5904 = PLANE ( 'NONE',  #9883 ) ;
#5905 = EDGE_CURVE ( 'NONE', #5954, #4916, #12861, .T. ) ;
#5906 = DIRECTION ( 'NONE',  ( 1.000000000000000000, 1.298018465182616140E-16, 0.000000000000000000 ) ) ;
#5907 = ORIENTED_EDGE ( 'NONE', *, *, #3459, .T. ) ;
#5908 = DIRECTION ( 'NONE',  ( 1.000000000000000000, 0.000000000000000000, -0.000000000000000000 ) ) ;
#5909 = ADVANCED_FACE ( 'NONE', ( #724, #11137 ), #12468, .F. ) ;
#5910 = CARTESIAN_POINT ( 'NONE',  ( 0.3137051932979792457, -3.805684345189695783, -13.20008686438109891 ) ) ;
#5911 = FACE_OUTER_BOUND ( 'NONE', #8521, .T. ) ;
#5912 = CARTESIAN_POINT ( 'NONE',  ( 0.3308579732647041749, 8.558831104907067555, -10.76782854710817716 ) ) ;
#5913 = DIRECTION ( 'NONE',  ( 0.4246593920385849930, 0.1376957914266804250, -0.8948208031649685923 ) ) ;
#5914 =( BOUNDED_SURFACE ( )  B_SPLINE_SURFACE ( 3, 1, ( 
 ( #14827, #17710 ),
 ( #600, #15214 ),
 ( #9387, #17992 ),
 ( #16561, #10635 ) ),
 .UNSPECIFIED., .F., .F., .T. ) 
 B_SPLINE_SURFACE_WITH_KNOTS ( ( 4, 4 ),
 ( 2, 2 ),
 ( 0.000000000000000000, 1.000000000000000000 ),
 ( 0.000000000000000000, 1.000000000000000000 ),
 .UNSPECIFIED. ) 
 GEOMETRIC_REPRESENTATION_ITEM ( )  RATIONAL_B_SPLINE_SURFACE ( (
 ( 1.000000000000000000, 1.000000000000000000),
 ( 0.9593108457356467333, 0.9995965569486454649),
 ( 0.9593108457356467333, 0.9995965569486454649),
 ( 1.000000000000000000, 1.000000000000000000) ) ) 
 REPRESENTATION_ITEM ( '' )  SURFACE ( )  );
#5915 = DIRECTION ( 'NONE',  ( 0.000000000000000000, 0.000000000000000000, 1.000000000000000000 ) ) ;
#5916 = VERTEX_POINT ( 'NONE', #10959 ) ;
#5917 = CIRCLE ( 'NONE', #12343, 16.06066017081991149 ) ;
#5918 = B_SPLINE_CURVE_WITH_KNOTS ( 'NONE', 3,
 ( #16874, #13732, #6754, #10877, #3777, #6472, #5302, #18125, #5026, #6663, #9434, #3876, #13908 ),
 .UNSPECIFIED., .F., .F.,
 ( 4, 3, 3, 3, 4 ),
 ( 3.878959614448864246E-18, 0.0002299780670421069050, 0.0004599561239687931019, 0.0006896788984287867625, 0.0009194956271626391958 ),
 .UNSPECIFIED. ) ;
#5919 = CARTESIAN_POINT ( 'NONE',  ( 0.3095370825347224519, 12.91933430393608084, 4.681152801286204479 ) ) ;
#5920 = CARTESIAN_POINT ( 'NONE',  ( 2.636624412715093513, -14.14563173255330142, 7.605649742761597665 ) ) ;
#5922 = VERTEX_POINT ( 'NONE', #13805 ) ;
#5921 = LINE ( 'NONE', #3237, #3868 ) ;
#5923 = CARTESIAN_POINT ( 'NONE',  ( 16.56679352167444819, 0.001518074900131727951, 0.009170718284672568082 ) ) ;
#5924 = ADVANCED_FACE ( 'NONE', ( #16960 ), #9594, .F. ) ;
#5925 = DIRECTION ( 'NONE',  ( -0.7635533937278216055, -0.5095610256143884298, 0.3966532189476580372 ) ) ;
#5926 = VERTEX_POINT ( 'NONE', #12378 ) ;
#5927 = EDGE_CURVE ( 'NONE', #10089, #8935, #11058, .T. ) ;
#5928 = CARTESIAN_POINT ( 'NONE',  ( 1.846524061778021419, 9.853584647934384932, 7.597197846158115553 ) ) ;
#5929 = UNCERTAINTY_MEASURE_WITH_UNIT (LENGTH_MEASURE( 1.000000000000000082E-05 ), #1487, 'distance_accuracy_value', 'NONE');
#5930 = ORIENTED_EDGE ( 'NONE', *, *, #12232, .F. ) ;
#5931 = CARTESIAN_POINT ( 'NONE',  ( 0.3170788640506440603, -4.392045232375903829, 13.02120094575826670 ) ) ;
#5932 = AXIS2_PLACEMENT_3D ( 'NONE', #8386, #5785, #17359 ) ;
#5933 = CARTESIAN_POINT ( 'NONE',  ( 0.4754618798421167414, -7.564402563418384240, -11.68486377711974811 ) ) ;
#5934 = CARTESIAN_POINT ( 'NONE',  ( 3.943463214271659518E-15, -27.00000000000000000, 22.91316734529526045 ) ) ;
#5935 = DIRECTION ( 'NONE',  ( 2.891205793294679312E-16, 1.000000000000000000, 0.000000000000000000 ) ) ;
#5936 = AXIS2_PLACEMENT_3D ( 'NONE', #18013, #16759, #13792 ) ;
#5937 = SURFACE_STYLE_FILL_AREA ( #10440 ) ;
#5938 = CARTESIAN_POINT ( 'NONE',  ( 2.002547531651519996, -10.57595306287287329, -6.845637710436306200 ) ) ;
#5939 = CARTESIAN_POINT ( 'NONE',  ( 3.950837973638668288, 0.000000000000000000, 0.000000000000000000 ) ) ;
#5940 = CARTESIAN_POINT ( 'NONE',  ( 0.3058872367615230181, -4.821066432589238282, -12.87003593440633331 ) ) ;
#5941 = CARTESIAN_POINT ( 'NONE',  ( 0.8740779401507028368, 12.04241618260048696, 7.708543377337672808 ) ) ;
#5942 = CARTESIAN_POINT ( 'NONE',  ( 2.123976203522053297, 15.26039569100264082, -3.347755036805743600 ) ) ;
#5943 = EDGE_CURVE ( 'NONE', #10455, #14367, #15247, .T. ) ;
#5944 =( REPRESENTATION_RELATIONSHIP ('NONE','NONE', #5200, #5797 ) REPRESENTATION_RELATIONSHIP_WITH_TRANSFORMATION ( #11041 )SHAPE_REPRESENTATION_RELATIONSHIP( ) );
#5945 = CIRCLE ( 'NONE', #17552, 2.600000000000039613 ) ;
#5946 = ORIENTED_EDGE ( 'NONE', *, *, #13616, .T. ) ;
#5947 = CARTESIAN_POINT ( 'NONE',  ( 16.58200780006414732, 0.004047297414157893791, 0.01041078477703983804 ) ) ;
#5948 = CARTESIAN_POINT ( 'NONE',  ( 2.636624412715384391, -11.60464335004044223, -11.10302021258006278 ) ) ;
#5949 = AXIS2_PLACEMENT_3D ( 'NONE', #18581, #13229, #337 ) ;
#5950 = VERTEX_POINT ( 'NONE', #3869 ) ;
#5951 = VECTOR ( 'NONE', #7364, 1000.000000000000000 ) ;
#5952 = ORIENTED_EDGE ( 'NONE', *, *, #15150, .T. ) ;
#5953 = CARTESIAN_POINT ( 'NONE',  ( 0.4862570985993235340, -13.44146924561383827, 3.580942890621619412 ) ) ;
#5954 = VERTEX_POINT ( 'NONE', #2422 ) ;
#5955 = CYLINDRICAL_SURFACE ( 'NONE', #6494, 2.499999999999992006 ) ;
#5956 = ORIENTED_EDGE ( 'NONE', *, *, #16056, .F. ) ;
#5957 = DIRECTION ( 'NONE',  ( 0.000000000000000000, 0.000000000000000000, -1.000000000000000000 ) ) ;
#5958 = B_SPLINE_CURVE_WITH_KNOTS ( 'NONE', 3,
 ( #9359, #13664, #12229, #10796, #15191, #2103, #7940, #13750, #662, #12315, #9535, #15545, #12496 ),
 .UNSPECIFIED., .F., .F.,
 ( 4, 3, 3, 3, 4 ),
 ( 0.000000000000000000, 0.0002299804304191505879, 0.0004599608082120279365, 0.0006467586077648024507, 0.0008336169836825989407 ),
 .UNSPECIFIED. ) ;
#5959 = CARTESIAN_POINT ( 'NONE',  ( 0.3150686449036029235, -13.73846184595214304, 0.1533607327085267646 ) ) ;
#5960 = CARTESIAN_POINT ( 'NONE',  ( 1.342453679581834924, 3.649820028552932971, -14.34050741580202981 ) ) ;
#5961 = CARTESIAN_POINT ( 'NONE',  ( 4.176146106109656457E-15, -27.00000000000000000, 29.01316734529526187 ) ) ;
#5962 = UNCERTAINTY_MEASURE_WITH_UNIT (LENGTH_MEASURE( 1.000000000000000082E-05 ), #7202, 'distance_accuracy_value', 'NONE');
#5963 = COLOUR_RGB ( '', 0.72549020, 0.75294118, 0.79215686) ;
#5964 = CARTESIAN_POINT ( 'NONE',  ( 0.3720661004400040439, 12.89739157014199833, -4.951033743989506242 ) ) ;
#5965 = CARTESIAN_POINT ( 'NONE',  ( 2.636624412716913390, 14.14563173255587536, -7.605649742760633991 ) ) ;
#5966 = AXIS2_PLACEMENT_3D ( 'NONE', #8128, #3718, #13940 ) ;
#5967 = B_SPLINE_CURVE_WITH_KNOTS ( 'NONE', 3,
 ( #2414, #3855, #7276, #5623, #15955, #9588 ),
 .UNSPECIFIED., .F., .F.,
 ( 4, 2, 4 ),
 ( 9.263427422397552964E-19, 0.001500839035891551789, 0.003001678071783102711 ),
 .UNSPECIFIED. ) ;
#5968 = PRESENTATION_STYLE_ASSIGNMENT (( #16302 ) ) ;
#5969 = CARTESIAN_POINT ( 'NONE',  ( 16.56872352241294521, -0.001821578298044716857, -0.01027347319884440967 ) ) ;
#5970 = CARTESIAN_POINT ( 'NONE',  ( 0.3308579732647007887, -10.76782854710821269, -8.558831104907037357 ) ) ;
#5971 = CARTESIAN_POINT ( 'NONE',  ( 0.3170788640506440603, -11.20690911610909168, 7.952793437297537515 ) ) ;
#5972 = CARTESIAN_POINT ( 'NONE',  ( 0.3151926232592509591, 13.73922722301401400, -0.07678256780562460471 ) ) ;
#5973 = EDGE_CURVE ( 'NONE', #9042, #18187, #3960, .T. ) ;
#5974 = EDGE_CURVE ( 'NONE', #18680, #3148, #5402, .T. ) ;
#5975 = EDGE_CURVE ( 'NONE', #11936, #14717, #635, .T. ) ;
#5976 = CARTESIAN_POINT ( 'NONE',  ( 1.846138399168762101, -11.95493567637852905, 3.446241763652952539 ) ) ;
#5977 = CARTESIAN_POINT ( 'NONE',  ( 16.57778382496167424, -0.007244066302946679421, -0.01306626476309297180 ) ) ;
#5978 = ORIENTED_EDGE ( 'NONE', *, *, #13531, .T. ) ;
#5979 = ORIENTED_EDGE ( 'NONE', *, *, #2923, .T. ) ;
#5980 = ORIENTED_EDGE ( 'NONE', *, *, #16025, .T. ) ;
#5981 = CIRCLE ( 'NONE', #1411, 16.06066017081991149 ) ;
#5982 = ORIENTED_EDGE ( 'NONE', *, *, #3436, .T. ) ;
#5983 =( GEOMETRIC_REPRESENTATION_CONTEXT ( 3 ) GLOBAL_UNCERTAINTY_ASSIGNED_CONTEXT ( ( #8993 ) ) GLOBAL_UNIT_ASSIGNED_CONTEXT ( ( #16404, #146, #2989 ) ) REPRESENTATION_CONTEXT ( 'NONE', 'WORKASPACE' ) );
#5984 = B_SPLINE_CURVE_WITH_KNOTS ( 'NONE', 3,
 ( #9205, #6630, #8068, #7979, #793, #12449 ),
 .UNSPECIFIED., .F., .F.,
 ( 4, 2, 4 ),
 ( 3.436766974507050665E-17, 0.0001825746017570568534, 0.0003651492035140793376 ),
 .UNSPECIFIED. ) ;
#5985 = CARTESIAN_POINT ( 'NONE',  ( 0.000000000000000000, 3.061616997868383141E-16, -2.500000000000000000 ) ) ;
#5986 = CARTESIAN_POINT ( 'NONE',  ( 1.846138399168762989, 10.30487220521570357, 6.971848976711047641 ) ) ;
#5987 = CARTESIAN_POINT ( 'NONE',  ( 16.56753206892534891, 0.009369540855502532517, -0.001549402974394196693 ) ) ;
#5988 = ORIENTED_EDGE ( 'NONE', *, *, #6353, .F. ) ;
#5989 = CARTESIAN_POINT ( 'NONE',  ( -33.49999999999999289, -12.50000000000000178, 0.000000000000000000 ) ) ;
#5990 = DIRECTION ( 'NONE',  ( -1.000000000000000000, -0.000000000000000000, -0.000000000000000000 ) ) ;
#5991 = DIRECTION ( 'NONE',  ( 0.000000000000000000, 0.000000000000000000, 1.000000000000000000 ) ) ;
#5992 = LINE ( 'NONE', #5887, #7683 ) ;
#5993 = LINE ( 'NONE', #4567, #4257 ) ;
#5994 = CARTESIAN_POINT ( 'NONE',  ( 1.847247051441592625, 11.88474976472817701, -3.685275815977066216 ) ) ;
#5995 = CARTESIAN_POINT ( 'NONE',  ( 16.56872352241294521, 0.001442253899401802278, 0.01033355228142402403 ) ) ;
#5996 = CARTESIAN_POINT ( 'NONE',  ( 0.3142014840576500267, -10.88517824918537080, -8.382000553815572630 ) ) ;
#5997 =( GEOMETRIC_REPRESENTATION_CONTEXT ( 3 ) GLOBAL_UNCERTAINTY_ASSIGNED_CONTEXT ( ( #41 ) ) GLOBAL_UNIT_ASSIGNED_CONTEXT ( ( #17046, #4042, #9689 ) ) REPRESENTATION_CONTEXT ( 'NONE', 'WORKASPACE' ) );
#5998 = CARTESIAN_POINT ( 'NONE',  ( 0.3148208552358953138, -8.260375059853256374, -10.97826876274321428 ) ) ;
#5999 = ORIENTED_EDGE ( 'NONE', *, *, #5118, .T. ) ;
#6000 = B_SPLINE_CURVE_WITH_KNOTS ( 'NONE', 3,
 ( #15991, #12937, #12493, #17239, #12841, #18766, #18666 ),
 .UNSPECIFIED., .F., .F.,
 ( 4, 3, 4 ),
 ( 3.198396408832238080E-18, 0.0002299780670421062274, 0.0004597478348664300451 ),
 .UNSPECIFIED. ) ;
#6001 =( BOUNDED_SURFACE ( )  B_SPLINE_SURFACE ( 3, 1, ( 
 ( #14702, #1525 ),
 ( #14415, #10215 ),
 ( #11750, #12888 ),
 ( #18714, #10197 ) ),
 .UNSPECIFIED., .F., .F., .T. ) 
 B_SPLINE_SURFACE_WITH_KNOTS ( ( 4, 4 ),
 ( 2, 2 ),
 ( 0.000000000000000000, 1.000000000000000000 ),
 ( 0.000000000000000000, 1.000000000000000000 ),
 .UNSPECIFIED. ) 
 GEOMETRIC_REPRESENTATION_ITEM ( )  RATIONAL_B_SPLINE_SURFACE ( (
 ( 1.000000000000000000, 1.000000000000000000),
 ( 0.7792777138730160313, 0.9689936506012927220),
 ( 0.7792777138730160313, 0.9689936506012927220),
 ( 1.000000000000000000, 1.000000000000000000) ) ) 
 REPRESENTATION_ITEM ( '' )  SURFACE ( )  );
#6002 = VERTEX_POINT ( 'NONE', #7913 ) ;
#6003 = ORIENTED_EDGE ( 'NONE', *, *, #3159, .F. ) ;
#6004 = ADVANCED_FACE ( 'NONE', ( #11051 ), #12287, .T. ) ;
#6005 = AXIS2_PLACEMENT_3D ( 'NONE', #12810, #5453, #7185 ) ;
#6006 = EDGE_LOOP ( 'NONE', ( #13152, #16508, #9386, #1416 ) ) ;
#6007 = B_SPLINE_CURVE_WITH_KNOTS ( 'NONE', 3,
 ( #5920, #1443, #17301, #13283, #2950, #8798 ),
 .UNSPECIFIED., .F., .F.,
 ( 4, 2, 4 ),
 ( 0.000000000000000000, 0.001656992708822777310, 0.003313985417645554619 ),
 .UNSPECIFIED. ) ;
#6008 = CARTESIAN_POINT ( 'NONE',  ( 16.56872352241294521, -0.007240717549633937135, 0.007512283835805527027 ) ) ;
#6009 = EDGE_CURVE ( 'NONE', #16688, #2315, #5126, .T. ) ;
#6010 = VECTOR ( 'NONE', #10977, 1000.000000000000000 ) ;
#6011 = VECTOR ( 'NONE', #4976, 1000.000000000000114 ) ;
#6012 = EDGE_LOOP ( 'NONE', ( #5364, #12185, #4556, #13125 ) ) ;
#6013 = CARTESIAN_POINT ( 'NONE',  ( 1.847461586945732703, 11.84459954310610463, 3.813310247068479431 ) ) ;
#6014 = CARTESIAN_POINT ( 'NONE',  ( 2.123976203522053297, 14.31368049382969687, 6.261444813538606269 ) ) ;
#6015 = AXIS2_PLACEMENT_3D ( 'NONE', #9059, #14427, #365 ) ;
#6016 = CARTESIAN_POINT ( 'NONE',  ( 0.000000000000000000, 0.000000000000000000, 5.000000000000000000 ) ) ;
#6017 = ORIENTED_EDGE ( 'NONE', *, *, #949, .F. ) ;
#6018 = DIRECTION ( 'NONE',  ( -0.7561779333270775005, -0.4122479608995667788, -0.5081796452863290847 ) ) ;
#6019 = EDGE_CURVE ( 'NONE', #4916, #11838, #8762, .T. ) ;
#6020 = LINE ( 'NONE', #10513, #15988 ) ;
#6021 = FACE_OUTER_BOUND ( 'NONE', #3392, .T. ) ;
#6022 = CARTESIAN_POINT ( 'NONE',  ( -1.500000000000001332, 6.799999999999999822, 5.000000000000000000 ) ) ;
#6023 = CARTESIAN_POINT ( 'NONE',  ( 1.977228804421969688, 1.488378900182327991, 15.33060379559086073 ) ) ;
#6024 = SURFACE_STYLE_USAGE ( .BOTH. , #17588 ) ;
#6025 = VECTOR ( 'NONE', #13501, 1000.000000000000227 ) ;
#6026 = B_SPLINE_CURVE_WITH_KNOTS ( 'NONE', 3,
 ( #6211, #16453, #16546, #6023, #17691, #8979 ),
 .UNSPECIFIED., .F., .F.,
 ( 4, 2, 4 ),
 ( 5.421010862427522170E-20, 0.001657017934710529891, 0.003314035869421059783 ),
 .UNSPECIFIED. ) ;
#6027 = VECTOR ( 'NONE', #7888, 1000.000000000000000 ) ;
#6028 = DIRECTION ( 'NONE',  ( -1.000000000000000000, 0.000000000000000000, 0.000000000000000000 ) ) ;
#6029 = ORIENTED_EDGE ( 'NONE', *, *, #12850, .F. ) ;
#6030 = ADVANCED_FACE ( 'NONE', ( #14554 ), #18526, .T. ) ;
#6031 = CARTESIAN_POINT ( 'NONE',  ( 1.254255976357533831, -13.61551404021209777, -5.487601330835152780 ) ) ;
#6033 = EDGE_LOOP ( 'NONE', ( #15992, #14556 ) ) ;
#6032 = LINE ( 'NONE', #4398, #17935 ) ;
#6034 = CARTESIAN_POINT ( 'NONE',  ( 0.3150692679895986115, 8.199139630396166112, -11.02465386701219252 ) ) ;
#6035 = EDGE_CURVE ( 'NONE', #10362, #2855, #1082, .T. ) ;
#6036 = ADVANCED_FACE ( 'NONE', ( #18855 ), #17848, .F. ) ;
#6037 = CARTESIAN_POINT ( 'NONE',  ( 16.56822296793089322, -0.007741272030791128758, -0.006547366384935482571 ) ) ;
#6038 = AXIS2_PLACEMENT_3D ( 'NONE', #14785, #13451, #7543 ) ;
#6039 = VERTEX_POINT ( 'NONE', #11510 ) ;
#6040 = CYLINDRICAL_SURFACE ( 'NONE', #13619, 2.600000000000092015 ) ;
#6041 = CARTESIAN_POINT ( 'NONE',  ( 5.872941918983158871, -7.500000000000001776, -12.71526091932864766 ) ) ;
#6042 = ORIENTED_EDGE ( 'NONE', *, *, #3192, .T. ) ;
#6043 = CARTESIAN_POINT ( 'NONE',  ( 1.847461586945732703, 3.813310247068605552, -11.84459954310606378 ) ) ;
#6044 = B_SPLINE_CURVE_WITH_KNOTS ( 'NONE', 3,
 ( #8986, #14814, #1726, #7577 ),
 .UNSPECIFIED., .F., .F.,
 ( 4, 4 ),
 ( 1.140836248210248932E-17, 0.003005512676784841391 ),
 .UNSPECIFIED. ) ;
#6045 = CARTESIAN_POINT ( 'NONE',  ( 0.3137051932979792457, -7.698472063774386420, -11.37800749014139612 ) ) ;
#6046 = FACE_OUTER_BOUND ( 'NONE', #5024, .T. ) ;
#6047 = EDGE_CURVE ( 'NONE', #796, #1036, #116, .T. ) ;
#6048 = CIRCLE ( 'NONE', #2671, 2.499999999999999556 ) ;
#6049 =( LENGTH_UNIT ( ) NAMED_UNIT ( * ) SI_UNIT ( .MILLI., .METRE. ) );
#6050 = CARTESIAN_POINT ( 'NONE',  ( 0.3095370825347224519, -7.700448427571790155, -11.38092634279636961 ) ) ;
#6051 = DIRECTION ( 'NONE',  ( -0.000000000000000000, -0.000000000000000000, 1.000000000000000000 ) ) ;
#6052 = CARTESIAN_POINT ( 'NONE',  ( 16.57210152137263393, -0.0006600038696347039187, 0.01453130299868522074 ) ) ;
#6053 = CARTESIAN_POINT ( 'NONE',  ( 2.747332970342022840, 2.409922051470680060, 16.17136872824899285 ) ) ;
#6054 = CARTESIAN_POINT ( 'NONE',  ( 0.3939822652208154752, 7.545099438012025317, 11.57634296752770453 ) ) ;
#6055 = ORIENTED_EDGE ( 'NONE', *, *, #6489, .F. ) ;
#6056 = DIRECTION ( 'NONE',  ( 0.000000000000000000, 0.000000000000000000, 1.000000000000000000 ) ) ;
#6057 = CARTESIAN_POINT ( 'NONE',  ( 16.56679352167444819, 0.008311568981097328460, -0.004162264567719685220 ) ) ;
#6058 = AXIS2_PLACEMENT_3D ( 'NONE', #10555, #16387, #17727 ) ;
#6059 = ORIENTED_EDGE ( 'NONE', *, *, #1544, .F. ) ;
#6060 = ORIENTED_EDGE ( 'NONE', *, *, #5746, .T. ) ;
#6061 = DIRECTION ( 'NONE',  ( 0.000000000000000000, 0.000000000000000000, -1.000000000000000000 ) ) ;
#6062 = ORIENTED_EDGE ( 'NONE', *, *, #14577, .F. ) ;
#6063 = DIRECTION ( 'NONE',  ( 0.000000000000000000, 0.000000000000000000, -1.000000000000000000 ) ) ;
#6064 = EDGE_LOOP ( 'NONE', ( #12244, #10378, #10510, #4503 ) ) ;
#6065 = EDGE_CURVE ( 'NONE', #1343, #8373, #17231, .T. ) ;
#6066 = CARTESIAN_POINT ( 'NONE',  ( 1.847380140988738484, 10.00162556679661741, -7.402792205948994564 ) ) ;
#6067 =( NAMED_UNIT ( * ) PLANE_ANGLE_UNIT ( ) SI_UNIT ( $, .RADIAN. ) );
#6068 = CARTESIAN_POINT ( 'NONE',  ( 0.000000000000000000, 0.000000000000000000, 0.000000000000000000 ) ) ;
#6069 = CARTESIAN_POINT ( 'NONE',  ( 0.3150692679896004988, 4.099798979280845579, 13.11337225490253644 ) ) ;
#6070 = EDGE_CURVE ( 'NONE', #15029, #18593, #16972, .T. ) ;
#6071 = CARTESIAN_POINT ( 'NONE',  ( 0.3095370825347233956, 12.91933430393614302, -4.681152801286028620 ) ) ;
#6072 = CARTESIAN_POINT ( 'NONE',  ( 3.950837973638676281, -6.316429227969383220, -13.10350451991847009 ) ) ;
#6073 =( NAMED_UNIT ( * ) PLANE_ANGLE_UNIT ( ) SI_UNIT ( $, .RADIAN. ) );
#6074 = CARTESIAN_POINT ( 'NONE',  ( 16.57778382496167424, -0.01306626476309383916, -0.007244066302947642193 ) ) ;
#6075 = CARTESIAN_POINT ( 'NONE',  ( 25.00000000000000000, -2.500000000000000444, -16.99999999999999645 ) ) ;
#6076 = APPLICATION_CONTEXT ( 'automotive_design' ) ;
#6077 = CARTESIAN_POINT ( 'NONE',  ( 2.636624412715137922, 2.161493821597615828, 15.91454522070216093 ) ) ;
#6078 = CYLINDRICAL_SURFACE ( 'NONE', #13346, 2.500000000000000000 ) ;
#6079 = CARTESIAN_POINT ( 'NONE',  ( 3.950837973638668288, 0.000000000000000000, 0.000000000000000000 ) ) ;
#6080 = VECTOR ( 'NONE', #5462, 1000.000000000000000 ) ;
#6081 = VERTEX_POINT ( 'NONE', #13122 ) ;
#6082 = ORIENTED_EDGE ( 'NONE', *, *, #16834, .F. ) ;
#6083 = ORIENTED_EDGE ( 'NONE', *, *, #14312, .T. ) ;
#6084 = ORIENTED_EDGE ( 'NONE', *, *, #7744, .T. ) ;
#6085 = CARTESIAN_POINT ( 'NONE',  ( 2.002547531651519996, 6.845637710436341727, -10.57595306287284842 ) ) ;
#6086 = CARTESIAN_POINT ( 'NONE',  ( 16.56822296793089322, -0.01011126603341003585, -0.0007467251401289729364 ) ) ;
#6087 = CARTESIAN_POINT ( 'NONE',  ( 1.846138399168762101, 0.4167076046097279440, -12.43476674860266051 ) ) ;
#6088 = EDGE_LOOP ( 'NONE', ( #7357, #3934, #4703 ) ) ;
#6089 = FACE_OUTER_BOUND ( 'NONE', #18388, .T. ) ;
#6090 = ADVANCED_FACE ( 'NONE', ( #17329 ), #12729, .T. ) ;
#6091 = EDGE_CURVE ( 'NONE', #2604, #15937, #1130, .T. ) ;
#6092 = CARTESIAN_POINT ( 'NONE',  ( 3.074695600507274307, 11.23985886659449029, -10.75417554975685341 ) ) ;
#6093 = ADVANCED_FACE ( 'NONE', ( #9864 ), #5846, .T. ) ;
#6094 = EDGE_LOOP ( 'NONE', ( #3238, #10792 ) ) ;
#6095 = CARTESIAN_POINT ( 'NONE',  ( 3.950837973638675393, 10.05648675950126325, 10.51028938476221342 ) ) ;
#6096 = CARTESIAN_POINT ( 'NONE',  ( 3.074695600507272086, 15.41438262616223298, -2.093687500612007923 ) ) ;
#6097 = CARTESIAN_POINT ( 'NONE',  ( 1.846613052777651198, 12.43780859207240042, -0.3401093050882249558 ) ) ;
#6098 = AXIS2_PLACEMENT_3D ( 'NONE', #10220, #9079, #7369 ) ;
#6099 = VECTOR ( 'NONE', #18441, 1000.000000000000114 ) ;
#6100 = CARTESIAN_POINT ( 'NONE',  ( 3.512766787570980931, 13.55823433651926280, 6.535475144496921907 ) ) ;
#6101 = CARTESIAN_POINT ( 'NONE',  ( 0.8740764193768004731, -5.211550415969136374, 13.31469591265773289 ) ) ;
#6102 = FACE_OUTER_BOUND ( 'NONE', #8541, .T. ) ;
#6103 = DIRECTION ( 'NONE',  ( -0.9868927730424200684, 9.023625820427603063E-27, -0.1613773668041546261 ) ) ;
#6104 = CARTESIAN_POINT ( 'NONE',  ( 0.3137051932979792457, 4.679953077377670745, -12.91601973349265720 ) ) ;
#6105 = VERTEX_POINT ( 'NONE', #7022 ) ;
#6106 = ORIENTED_EDGE ( 'NONE', *, *, #15840, .F. ) ;
#6107 = ORIENTED_EDGE ( 'NONE', *, *, #13982, .T. ) ;
#6108 = ORIENTED_EDGE ( 'NONE', *, *, #11257, .F. ) ;
#6109 = EDGE_CURVE ( 'NONE', #11553, #8437, #3285, .T. ) ;
#6110 = LINE ( 'NONE', #1905, #8606 ) ;
#6111 = ORIENTED_EDGE ( 'NONE', *, *, #13692, .T. ) ;
#6112 = LINE ( 'NONE', #9625, #12057 ) ;
#6113 = CARTESIAN_POINT ( 'NONE',  ( 1.847372867223028070, 11.80112642014554325, 3.945260592619082907 ) ) ;
#6114 = DIRECTION ( 'NONE',  ( 0.000000000000000000, -1.000000000000000000, 0.000000000000000000 ) ) ;
#6115 = CARTESIAN_POINT ( 'NONE',  ( 2.697797270744668463, 0.9169917281809109033, -13.26309265156976203 ) ) ;
#6116 = EDGE_LOOP ( 'NONE', ( #4838, #18191, #13790, #935 ) ) ;
#6117 = CARTESIAN_POINT ( 'NONE',  ( 1.847461586945727374, -3.813310247068524284, 11.84459954310609753 ) ) ;
#6118 = DIRECTION ( 'NONE',  ( -0.7635533937278216055, -0.2197766120036420967, -0.6071939193889598352 ) ) ;
#6119 = CARTESIAN_POINT ( 'NONE',  ( 2.002547531651519996, -7.942910686618240845, 9.778737580845669797 ) ) ;
#6120 = CARTESIAN_POINT ( 'NONE',  ( 16.56753206892534891, -0.009369540855502522109, 0.001549402974394263697 ) ) ;
#6121 = EDGE_CURVE ( 'NONE', #2897, #4902, #5112, .T. ) ;
#6122 = DIRECTION ( 'NONE',  ( 0.000000000000000000, 0.000000000000000000, -1.000000000000000000 ) ) ;
#6123 = CARTESIAN_POINT ( 'NONE',  ( 0.3137051932979792457, 13.20008686438105983, 3.805684345189833451 ) ) ;
#6124 = EDGE_CURVE ( 'NONE', #1472, #10380, #5781, .T. ) ;
#6125 =( BOUNDED_SURFACE ( )  B_SPLINE_SURFACE ( 3, 1, ( 
 ( #3933, #12996 ),
 ( #14254, #8419 ),
 ( #6896, #18450 ),
 ( #18548, #18636 ) ),
 .UNSPECIFIED., .F., .F., .T. ) 
 B_SPLINE_SURFACE_WITH_KNOTS ( ( 4, 4 ),
 ( 2, 2 ),
 ( 0.000000000000000000, 1.000000000000000000 ),
 ( 0.000000000000000000, 1.000000000000000000 ),
 .UNSPECIFIED. ) 
 GEOMETRIC_REPRESENTATION_ITEM ( )  RATIONAL_B_SPLINE_SURFACE ( (
 ( 1.000000000000000000, 1.000000000000000000),
 ( 0.7792777138730160313, 0.9689936506012927220),
 ( 0.7792777138730160313, 0.9689936506012927220),
 ( 1.000000000000000000, 1.000000000000000000) ) ) 
 REPRESENTATION_ITEM ( '' )  SURFACE ( )  );
#6126 = AXIS2_PLACEMENT_3D ( 'NONE', #16672, #2232, #3946 ) ;
#6127 = CARTESIAN_POINT ( 'NONE',  ( 0.3170788640506441158, 11.02668139258453905, -8.200855617524412722 ) ) ;
#6128 = VERTEX_POINT ( 'NONE', #12177 ) ;
#6129 = CYLINDRICAL_SURFACE ( 'NONE', #5820, 2.600000000000092015 ) ;
#6131 = EDGE_LOOP ( 'NONE', ( #3921, #2697, #16691, #7739, #9158, #3218 ) ) ;
#6130 = CARTESIAN_POINT ( 'NONE',  ( 0.3150686449036074199, 0.1533607327085746430, 13.73846184595213771 ) ) ;
#6132 = LINE ( 'NONE', #5066, #6011 ) ;
#6133 = CARTESIAN_POINT ( 'NONE',  ( 0.3137051932979809665, -4.679953077377580151, 12.91601973349268917 ) ) ;
#6134 = B_SPLINE_CURVE_WITH_KNOTS ( 'NONE', 3,
 ( #2598, #8627, #1364, #8442 ),
 .UNSPECIFIED., .F., .F.,
 ( 4, 4 ),
 ( 4.459867448574166155E-16, 0.002004993803842844771 ),
 .UNSPECIFIED. ) ;
#6135 = EDGE_LOOP ( 'NONE', ( #1413, #4514, #15613, #12384 ) ) ;
#6136 = CARTESIAN_POINT ( 'NONE',  ( 0.4862570985993252548, -12.97920246947875889, -5.003653737315625349 ) ) ;
#6137 = CARTESIAN_POINT ( 'NONE',  ( 3.329573251200529160, -7.500000000000264677, -13.21489263293670469 ) ) ;
#6138 = VERTEX_POINT ( 'NONE', #14840 ) ;
#6139 = CARTESIAN_POINT ( 'NONE',  ( 1.847034903785822246, 4.063013886994871982, -11.76058231742741533 ) ) ;
#6140 = CARTESIAN_POINT ( 'NONE',  ( 0.3095370825347233956, 13.73357284481724783, -0.4597470195090692657 ) ) ;
#6141 = LINE ( 'NONE', #11969, #14351 ) ;
#6142 = CARTESIAN_POINT ( 'NONE',  ( 1.254255976357772751, -11.25336128106935263, -9.426444230097215993 ) ) ;
#6143 = VECTOR ( 'NONE', #8776, 1000.000000000000000 ) ;
#6144 = EDGE_CURVE ( 'NONE', #9516, #13434, #9222, .T. ) ;
#6145 = VERTEX_POINT ( 'NONE', #16383 ) ;
#6146 = CARTESIAN_POINT ( 'NONE',  ( 1.846524061778018311, -10.27028962889602148, 7.023652644192237560 ) ) ;
#6147 = CARTESIAN_POINT ( 'NONE',  ( 2.369999999999999662, 0.000000000000000000, 0.000000000000000000 ) ) ;
#6148 = CARTESIAN_POINT ( 'NONE',  ( 1.918918678667072886, 0.6348738215465219437, 12.49849921341423453 ) ) ;
#6149 = CARTESIAN_POINT ( 'NONE',  ( 16.56679352167444819, 0.006618561353599204840, -0.006526964904752983153 ) ) ;
#6150 = CARTESIAN_POINT ( 'NONE',  ( 3.512766787571172333, 14.91422000116773994, 2.025881399556380469 ) ) ;
#6151 = ORIENTED_EDGE ( 'NONE', *, *, #7719, .T. ) ;
#6152 = CARTESIAN_POINT ( 'NONE',  ( 0.3145729642390375225, -3.952965287571204023, 13.15786090015082799 ) ) ;
#6153 = CARTESIAN_POINT ( 'NONE',  ( 0.3132635586635977298, -13.72732610560088418, 0.5277914263192632349 ) ) ;
#6154 = VERTEX_POINT ( 'NONE', #9115 ) ;
#6155 = VERTEX_POINT ( 'NONE', #14647 ) ;
#6157 = CARTESIAN_POINT ( 'NONE',  ( 0.3150692679895978343, 11.20465057551037091, -7.951395415074959061 ) ) ;
#6156 = VECTOR ( 'NONE', #3557, 1000.000000000000000 ) ;
#6158 = EDGE_CURVE ( 'NONE', #3822, #10095, #8311, .T. ) ;
#6159 = ORIENTED_EDGE ( 'NONE', *, *, #14290, .T. ) ;
#6160 = DIRECTION ( 'NONE',  ( -1.000000000000000000, 0.000000000000000000, 0.000000000000000000 ) ) ;
#6161 = ORIENTED_EDGE ( 'NONE', *, *, #13811, .T. ) ;
#6162 = CARTESIAN_POINT ( 'NONE',  ( 4.336808689942017736E-15, -30.00000000000000000, 31.00000000000000000 ) ) ;
#6163 = DIRECTION ( 'NONE',  ( 0.8629742774544855166, -0.5052478564545411777, 0.000000000000000000 ) ) ;
#6164 = DIRECTION ( 'NONE',  ( 1.000000000000000000, 0.000000000000000000, -0.000000000000000000 ) ) ;
#6165 = PRODUCT_DEFINITION_SHAPE ( 'NONE', 'NONE',  #6510 ) ;
#6166 = CARTESIAN_POINT ( 'NONE',  ( -58.82978549640777288, -10.68512861272758308, 3.000000000000000000 ) ) ;
#6167 = CARTESIAN_POINT ( 'NONE',  ( 1.342453679581834924, -0.9602753779831757486, 14.76648944001038899 ) ) ;
#6168 = DIRECTION ( 'NONE',  ( -1.000000000000000000, 0.000000000000000000, 0.000000000000000000 ) ) ;
#6169 = CARTESIAN_POINT ( 'NONE',  ( 2.636624412716062960, 6.973567714909310489, -14.46769361191320868 ) ) ;
#6170 = CARTESIAN_POINT ( 'NONE',  ( 1.562796894703937678, 3.061616997868383141E-16, -2.500000000000000000 ) ) ;
#6171 = LINE ( 'NONE', #4643, #2054 ) ;
#6172 = ADVANCED_FACE ( 'NONE', ( #8821 ), #4672, .F. ) ;
#6173 = B_SPLINE_CURVE_WITH_KNOTS ( 'NONE', 3,
 ( #2430, #16787, #9605, #14093, #1000, #11244, #17059 ),
 .UNSPECIFIED., .F., .F.,
 ( 4, 3, 4 ),
 ( 1.951563910473907981E-18, 0.0002299804304191482840, 0.0004168119862248656667 ),
 .UNSPECIFIED. ) ;
#6174 = CARTESIAN_POINT ( 'NONE',  ( 1.847461586945727596, -11.84459954310608332, -3.813310247068566028 ) ) ;
#6175 = AXIS2_PLACEMENT_3D ( 'NONE', #12791, #18617, #14129 ) ;
#6176 = CARTESIAN_POINT ( 'NONE',  ( 0.8740779401508861346, -14.27348745891575987, 0.8420120399581260129 ) ) ;
#6177 = ORIENTED_EDGE ( 'NONE', *, *, #10676, .T. ) ;
#6178 = ORIENTED_EDGE ( 'NONE', *, *, #130, .F. ) ;
#6179 = ORIENTED_EDGE ( 'NONE', *, *, #9306, .F. ) ;
#6180 = ORIENTED_EDGE ( 'NONE', *, *, #4580, .T. ) ;
#6181 = CARTESIAN_POINT ( 'NONE',  ( 0.3151926232592474619, -8.137833541809298410, -11.07013665200804198 ) ) ;
#6182 = CARTESIAN_POINT ( 'NONE',  ( 0.3095370825347233956, 10.84046130709070610, -8.444334731363889901 ) ) ;
#6183 = CARTESIAN_POINT ( 'NONE',  ( 1.918921323896323639, -3.258415356426438869, -12.08297777410668417 ) ) ;
#6184 = FACE_OUTER_BOUND ( 'NONE', #14679, .T. ) ;
#6185 = CARTESIAN_POINT ( 'NONE',  ( 2.636624412716061627, -7.605649742761058540, -14.14563173255469408 ) ) ;
#6186 = CARTESIAN_POINT ( 'NONE',  ( 0.3720661004400037664, 0.7231997263366731765, -13.79610186261028559 ) ) ;
#6187 = LINE ( 'NONE', #5129, #12544 ) ;
#6188 = CARTESIAN_POINT ( 'NONE',  ( 3.950837973638675393, -2.591948120961912849, 14.31366178983252446 ) ) ;
#6189 = CARTESIAN_POINT ( 'NONE',  ( 1.847412631396507798, 11.84727953344288132, -3.804043368582538776 ) ) ;
#6190 = CARTESIAN_POINT ( 'NONE',  ( 1.845755665166724402, -9.776700214453573068, -7.694641135842929636 ) ) ;
#6191 = DIRECTION ( 'NONE',  ( 1.000000000000000000, 0.000000000000000000, 0.000000000000000000 ) ) ;
#6192 = DIRECTION ( 'NONE',  ( 0.000000000000000000, 0.000000000000000000, 1.000000000000000000 ) ) ;
#6193 = CARTESIAN_POINT ( 'NONE',  ( 0.3145729642390374670, 3.952965287571295949, -13.15786090015079957 ) ) ;
#6194 = ORIENTED_EDGE ( 'NONE', *, *, #12538, .F. ) ;
#6195 = EDGE_LOOP ( 'NONE', ( #4307, #7067, #18702, #17886 ) ) ;
#6196 = EDGE_CURVE ( 'NONE', #11775, #15252, #7570, .T. ) ;
#6197 = ORIENTED_EDGE ( 'NONE', *, *, #10655, .F. ) ;
#6198 = ORIENTED_EDGE ( 'NONE', *, *, #8882, .T. ) ;
#6199 = DIRECTION ( 'NONE',  ( 0.000000000000000000, 0.000000000000000000, 1.000000000000000000 ) ) ;
#6200 = CARTESIAN_POINT ( 'NONE',  ( 1.977436885026404134, 10.21547824869624321, -11.52792723756320470 ) ) ;
#6201 = CARTESIAN_POINT ( 'NONE',  ( 16.56753206892534891, 0.009369540855502530782, -0.001549402974394192573 ) ) ;
#6202 = CARTESIAN_POINT ( 'NONE',  ( 16.56753206892534891, 0.001549402974393146101, -0.009369540855502138735 ) ) ;
#6203 = CARTESIAN_POINT ( 'NONE',  ( -27.32408120756002035, 20.00000000000000000, 0.000000000000000000 ) ) ;
#6204 = ORIENTED_EDGE ( 'NONE', *, *, #5672, .F. ) ;
#6205 = CARTESIAN_POINT ( 'NONE',  ( 0.4385251269669950269, -0.7363879510386354132, 13.84299131624729462 ) ) ;
#6206 = CIRCLE ( 'NONE', #11097, 2.600000000000039613 ) ;
#6207 = CARTESIAN_POINT ( 'NONE',  ( 16.56822296793089322, 0.008619100080559776930, 0.005339139727952691740 ) ) ;
#6208 = CARTESIAN_POINT ( 'NONE',  ( 16.58200780006414732, 0.004047297414157893791, 0.01041078477703983804 ) ) ;
#6209 = CARTESIAN_POINT ( 'NONE',  ( 2.002547531651519996, 11.75462648437101976, 4.532360870844369671 ) ) ;
#6210 = B_SPLINE_CURVE_WITH_KNOTS ( 'NONE', 3,
 ( #17514, #4620, #14455, #225, #15891, #4331 ),
 .UNSPECIFIED., .F., .F.,
 ( 4, 2, 4 ),
 ( 0.000000000000000000, 0.001500839035891551789, 0.003001678071783103578 ),
 .UNSPECIFIED. ) ;
#6211 = CARTESIAN_POINT ( 'NONE',  ( 0.4862570985993235340, 0.7479633556562450547, 13.89016912371017831 ) ) ;
#6212 =( LENGTH_UNIT ( ) NAMED_UNIT ( * ) SI_UNIT ( .MILLI., .METRE. ) );
#6213 =( REPRESENTATION_RELATIONSHIP ('NONE','NONE', #5200, #18049 ) REPRESENTATION_RELATIONSHIP_WITH_TRANSFORMATION ( #10150 )SHAPE_REPRESENTATION_RELATIONSHIP( ) );
#6214 = B_SPLINE_CURVE_WITH_KNOTS ( 'NONE', 3,
 ( #15000, #11950, #10519, #2943 ),
 .UNSPECIFIED., .F., .F.,
 ( 4, 4 ),
 ( 2.006682199098010609E-17, 0.003005512676784850064 ),
 .UNSPECIFIED. ) ;
#6215 = CARTESIAN_POINT ( 'NONE',  ( 0.3308579732647041749, 8.558831104907067555, -10.76782854710817716 ) ) ;
#6216 = VERTEX_POINT ( 'NONE', #228 ) ;
#6217 = EDGE_LOOP ( 'NONE', ( #8732, #16641, #16798, #3701 ) ) ;
#6218 = CARTESIAN_POINT ( 'NONE',  ( 0.8740764193766143997, 13.31469591265758545, 5.211550415968988936 ) ) ;
#6220 = ORIENTED_EDGE ( 'NONE', *, *, #3184, .T. ) ;
#6219 = CARTESIAN_POINT ( 'NONE',  ( 1.847426409206450959, 1.966388007708274189E-11, -12.44303504652081038 ) ) ;
#6221 = CARTESIAN_POINT ( 'NONE',  ( 15.00000000000000711, -19.99999999999999645, 7.000000000000000000 ) ) ;
#6222 = VECTOR ( 'NONE', #12669, 1000.000000000000114 ) ;
#6223 = EDGE_CURVE ( 'NONE', #8687, #11022, #11721, .T. ) ;
#6224 = EDGE_CURVE ( 'NONE', #14019, #14561, #6351, .T. ) ;
#6225 = DIRECTION ( 'NONE',  ( 0.000000000000000000, 0.000000000000000000, 1.000000000000000000 ) ) ;
#6226 = ORIENTED_EDGE ( 'NONE', *, *, #10681, .T. ) ;
#6227 = PLANE ( 'NONE',  #18489 ) ;
#6228 = CARTESIAN_POINT ( 'NONE',  ( -1.517261107235201356, -6.836011689345085962, -11.99999999467221912 ) ) ;
#6229 = ADVANCED_BREP_SHAPE_REPRESENTATION ( '', ( #16223, #2030 ), #8454 ) ;
#6230 = ORIENTED_EDGE ( 'NONE', *, *, #2678, .F. ) ;
#6231 = CARTESIAN_POINT ( 'NONE',  ( 1.847247051441591070, 4.004229874809190903, -11.78111530882019053 ) ) ;
#6232 = CARTESIAN_POINT ( 'NONE',  ( 2.705023505549867036, 0.8488853074252974418, 13.27418276223636440 ) ) ;
#6233 = CARTESIAN_POINT ( 'NONE',  ( 0.4385251269669945273, -7.540955776459655091, -11.63205320541531052 ) ) ;
#6234 = CARTESIAN_POINT ( 'NONE',  ( 2.747332970342022840, 14.63517873738956965, -7.289199830146954717 ) ) ;
#6235 = CIRCLE ( 'NONE', #2538, 5.000000000000000000 ) ;
#6236 = AXIS2_PLACEMENT_3D ( 'NONE', #674, #15466, #13846 ) ;
#6237 = ORIENTED_EDGE ( 'NONE', *, *, #6035, .T. ) ;
#6238 = PRODUCT_DEFINITION_FORMATION_WITH_SPECIFIED_SOURCE ( 'ANY', '', #3577, .NOT_KNOWN. ) ;
#6239 = CARTESIAN_POINT ( 'NONE',  ( 16.56872352241294521, 0.001442253899401220278, -0.01033355228142500415 ) ) ;
#6240 = CARTESIAN_POINT ( 'NONE',  ( 2.697797270744669795, 12.89731672021094511, -3.226410068829295597 ) ) ;
#6241 = DIRECTION ( 'NONE',  ( -1.000000000000000000, -0.000000000000000000, -0.000000000000000000 ) ) ;
#6243 = ORIENTED_EDGE ( 'NONE', *, *, #15577, .F. ) ;
#6242 = CARTESIAN_POINT ( 'NONE',  ( 2.636624412714236865, 0.000000000000000000, 0.000000000000000000 ) ) ;
#6244 = CARTESIAN_POINT ( 'NONE',  ( 1.846138399168762101, -10.30487220521565028, -6.971848976711123136 ) ) ;
#6245 = EDGE_LOOP ( 'NONE', ( #12307, #15035 ) ) ;
#6246 = CARTESIAN_POINT ( 'NONE',  ( 1.846138399168762989, 9.815003036200414144, 7.646096044339929954 ) ) ;
#6247 = CARTESIAN_POINT ( 'NONE',  ( 0.4862570985993235340, -10.79774104611366781, -8.769551628660854803 ) ) ;
#6248 = ORIENTED_EDGE ( 'NONE', *, *, #4112, .F. ) ;
#6249 = VERTEX_POINT ( 'NONE', #6246 ) ;
#6250 = DIRECTION ( 'NONE',  ( 0.000000000000000000, 0.000000000000000000, 1.000000000000000000 ) ) ;
#6251 = EDGE_CURVE ( 'NONE', #666, #1293, #10164, .T. ) ;
#6252 = ORIENTED_EDGE ( 'NONE', *, *, #8416, .F. ) ;
#6253 = DIRECTION ( 'NONE',  ( 0.000000000000000000, 0.000000000000000000, 1.000000000000000000 ) ) ;
#6254 = VECTOR ( 'NONE', #16165, 1000.000000000000114 ) ;
#6255 = EDGE_LOOP ( 'NONE', ( #2692, #11300 ) ) ;
#6256 = VECTOR ( 'NONE', #4295, 1000.000000000000114 ) ;
#6257 = CARTESIAN_POINT ( 'NONE',  ( 1.560000000000000053, -1.299038105676658450, 0.7500000000000007772 ) ) ;
#6258 = AXIS2_PLACEMENT_3D ( 'NONE', #14109, #6959, #11440 ) ;
#6259 = FACE_OUTER_BOUND ( 'NONE', #14478, .T. ) ;
#6260 = CARTESIAN_POINT ( 'NONE',  ( 16.56679352167444819, -0.001518074900131792136, -0.009170718284672557674 ) ) ;
#6261 = CARTESIAN_POINT ( 'NONE',  ( 16.57778382496167424, 0.01092721432669108844, -0.01018821665058837478 ) ) ;
#6262 = DIRECTION ( 'NONE',  ( 0.000000000000000000, -1.000000000000000000, 0.000000000000000000 ) ) ;
#6263 = CARTESIAN_POINT ( 'NONE',  ( 2.747332970342022840, 7.289199830147313541, -14.63517873738939379 ) ) ;
#6264 =( LENGTH_UNIT ( ) NAMED_UNIT ( * ) SI_UNIT ( .MILLI., .METRE. ) );
#6265 = CARTESIAN_POINT ( 'NONE',  ( 16.57778382496167424, -0.01466529584256673520, 0.002851818597093359019 ) ) ;
#6266 = DIRECTION ( 'NONE',  ( 2.081668171172168119E-15, 0.000000000000000000, 1.000000000000000000 ) ) ;
#6267 = AXIS2_PLACEMENT_3D ( 'NONE', #1044, #18542, #12805 ) ;
#6268 = AXIS2_PLACEMENT_3D ( 'NONE', #3282, #17929, #7804 ) ;
#6269 = CARTESIAN_POINT ( 'NONE',  ( 1.846822687350019754, 7.547953575784267066, -9.891732594446496662 ) ) ;
#6270 = VECTOR ( 'NONE', #7822, 1000.000000000000000 ) ;
#6271 = LINE ( 'NONE', #10764, #16074 ) ;
#6272 = PRODUCT_DEFINITION ( 'UNKNOWN', '', #15091, #18039 ) ;
#6273 = CARTESIAN_POINT ( 'NONE',  ( 2.750000000000000000, 0.000000000000000000, 2.700000000000000178 ) ) ;
#6274 = CARTESIAN_POINT ( 'NONE',  ( 0.4862570985993235340, -13.89016912371018186, 0.7479633556561964269 ) ) ;
#6275 = EDGE_CURVE ( 'NONE', #7476, #17964, #12448, .T. ) ;
#6276 = ORIENTED_EDGE ( 'NONE', *, *, #14821, .F. ) ;
#6277 = ORIENTED_EDGE ( 'NONE', *, *, #12050, .F. ) ;
#6278 = EDGE_CURVE ( 'NONE', #8470, #12351, #12667, .T. ) ;
#6279 = ORIENTED_EDGE ( 'NONE', *, *, #14146, .T. ) ;
#6280 = EDGE_LOOP ( 'NONE', ( #12272, #596, #10068, #14892 ) ) ;
#6281 = CARTESIAN_POINT ( 'NONE',  ( 0.3142011359265339254, 0.3830873813806325301, 13.73310835363014171 ) ) ;
#6282 = VECTOR ( 'NONE', #539, 1000.000000000000114 ) ;
#6283 = CARTESIAN_POINT ( 'NONE',  ( 0.3137051932979792457, -13.73004976592201842, -0.4596302728641207813 ) ) ;
#6284 = VECTOR ( 'NONE', #3507, 1000.000000000000114 ) ;
#6285 = DIRECTION ( 'NONE',  ( 1.000000000000000000, 0.000000000000000000, 0.000000000000000000 ) ) ;
#6286 = CARTESIAN_POINT ( 'NONE',  ( 2.705023505549867036, 0.8488853074252974418, 13.27418276223636440 ) ) ;
#6287 = CARTESIAN_POINT ( 'NONE',  ( 2.179449471770337432, -4.500000000000000000, -6.000000000000000000 ) ) ;
#6288 = B_SPLINE_CURVE_WITH_KNOTS ( 'NONE', 3,
 ( #5019, #16865, #6654, #5295, #5391, #9509 ),
 .UNSPECIFIED., .F., .F.,
 ( 4, 2, 4 ),
 ( 0.000000000000000000, 0.001500839035891550271, 0.003001678071783100542 ),
 .UNSPECIFIED. ) ;
#6289 = DIRECTION ( 'NONE',  ( 0.000000000000000000, 0.000000000000000000, 1.000000000000000000 ) ) ;
#6290 = CARTESIAN_POINT ( 'NONE',  ( 16.56872352241294521, -0.007240717549633937135, 0.007512283835805527027 ) ) ;
#6291 = CARTESIAN_POINT ( 'NONE',  ( 0.3095370825347234511, -8.444334731364085300, 10.84046130709055333 ) ) ;
#6292 = ADVANCED_FACE ( 'NONE', ( #15311 ), #8082, .F. ) ;
#6293 = DIRECTION ( 'NONE',  ( 0.7071067818211348444, 0.000000000000000000, -0.7071067805519601901 ) ) ;
#6294 = FACE_OUTER_BOUND ( 'NONE', #5042, .T. ) ;
#6295 = CARTESIAN_POINT ( 'NONE',  ( 3.950837973638675393, 10.05648675950126325, 10.51028938476221342 ) ) ;
#6296 = CARTESIAN_POINT ( 'NONE',  ( 0.3142014840576516921, 4.608051180497103161, -12.94260032291123785 ) ) ;
#6297 = EDGE_LOOP ( 'NONE', ( #2163, #11717, #8210, #11462 ) ) ;
#6298 = AXIS2_PLACEMENT_3D ( 'NONE', #16894, #9722, #9629 ) ;
#6299 = ORIENTED_EDGE ( 'NONE', *, *, #403, .F. ) ;
#6300 = ORIENTED_EDGE ( 'NONE', *, *, #16341, .F. ) ;
#6301 = VERTEX_POINT ( 'NONE', #16572 ) ;
#6302 = CARTESIAN_POINT ( 'NONE',  ( 1.847247051441588184, -7.177495230324629105, -10.16425585218608951 ) ) ;
#6303 = FACE_OUTER_BOUND ( 'NONE', #7291, .T. ) ;
#6304 = CARTESIAN_POINT ( 'NONE',  ( 1.560000000000000053, 0.8660254037844389297, -1.500000000000000000 ) ) ;
#6305 = CARTESIAN_POINT ( 'NONE',  ( -199.9999999999999716, 4.999999999999973355, 5.999999999999999112 ) ) ;
#6306 = B_SPLINE_CURVE_WITH_KNOTS ( 'NONE', 3,
 ( #13157, #17851, #10297, #14496, #1405, #169 ),
 .UNSPECIFIED., .F., .F.,
 ( 4, 2, 4 ),
 ( 3.337089043155729788E-17, 0.0001825746017570573684, 0.0003651492035140813976 ),
 .UNSPECIFIED. ) ;
#6307 = CARTESIAN_POINT ( 'NONE',  ( 2.320521194582547242, 1.795798718313595055, 15.64520804578271118 ) ) ;
#6308 = ORIENTED_EDGE ( 'NONE', *, *, #12102, .T. ) ;
#6309 = CARTESIAN_POINT ( 'NONE',  ( -5.051325721637062394, 7.500000000000000000, -16.81741242948696069 ) ) ;
#6310 = CYLINDRICAL_SURFACE ( 'NONE', #10182, 7.000000000000000000 ) ;
#6311 = CARTESIAN_POINT ( 'NONE',  ( -6.118503526524619041, 3.404981712888209611, -11.99999999938683892 ) ) ;
#6312 = FACE_OUTER_BOUND ( 'NONE', #3892, .T. ) ;
#6313 = PRESENTATION_LAYER_ASSIGNMENT (  '', '', ( #9367 ) ) ;
#6314 = CARTESIAN_POINT ( 'NONE',  ( 0.000000000000000000, 0.000000000000000000, -6.000000000000000000 ) ) ;
#6315 = EDGE_CURVE ( 'NONE', #4723, #78, #1992, .T. ) ;
#6316 = CARTESIAN_POINT ( 'NONE',  ( 2.002547531651519996, -6.845637710436264456, 10.57595306287289638 ) ) ;
#6317 = CARTESIAN_POINT ( 'NONE',  ( 0.3148208552358952583, 12.99355031785211168, -4.463611911212083783 ) ) ;
#6318 = ORIENTED_EDGE ( 'NONE', *, *, #7855, .F. ) ;
#6319 = CIRCLE ( 'NONE', #16987, 5.000000000000004441 ) ;
#6320 = DIRECTION ( 'NONE',  ( -0.9034263296138832500, 0.000000000000000000, -0.4287433579198481337 ) ) ;
#6322 = ORIENTED_EDGE ( 'NONE', *, *, #2848, .F. ) ;
#6321 = CARTESIAN_POINT ( 'NONE',  ( 3.950837973638668288, 0.000000000000000000, 0.000000000000000000 ) ) ;
#6323 = DIRECTION ( 'NONE',  ( -0.000000000000000000, -0.000000000000000000, -1.000000000000000000 ) ) ;
#6324 = VECTOR ( 'NONE', #15842, 1000.000000000000000 ) ;
#6325 = VECTOR ( 'NONE', #3167, 1000.000000000000000 ) ;
#6326 = CARTESIAN_POINT ( 'NONE',  ( 0.3132635586635977853, 10.79541209008116454, -8.495712071659280440 ) ) ;
#6327 = STYLED_ITEM ( 'NONE', ( #16836 ), #556 ) ;
#6328 = AXIS2_PLACEMENT_3D ( 'NONE', #12823, #15882, #18649 ) ;
#6329 = ORIENTED_EDGE ( 'NONE', *, *, #12050, .T. ) ;
#6330 = DIRECTION ( 'NONE',  ( 0.000000000000000000, 0.000000000000000000, -1.000000000000000000 ) ) ;
#6331 = PRODUCT_DEFINITION_SHAPE ( 'NONE', 'NONE',  #3089 ) ;
#6332 = CARTESIAN_POINT ( 'NONE',  ( 0.2286586286997084050, -7.499999999999928946, -13.03338879287354679 ) ) ;
#6333 = ORIENTED_EDGE ( 'NONE', *, *, #2128, .F. ) ;
#6334 = CARTESIAN_POINT ( 'NONE',  ( 3.377929128793396352, -12.02809354424095822, -7.136734442940969814 ) ) ;
#6335 = CARTESIAN_POINT ( 'NONE',  ( 16.58200780006414732, -0.006043560077721639792, -0.009393638146079824613 ) ) ;
#6336 = AXIS2_PLACEMENT_3D ( 'NONE', #11237, #12649, #8000 ) ;
#6337 = LINE ( 'NONE', #5934, #16471 ) ;
#6338 = DIRECTION ( 'NONE',  ( 1.000000000000000000, 0.000000000000000000, -0.000000000000000000 ) ) ;
#6339 = AXIS2_PLACEMENT_3D ( 'NONE', #17346, #14200, #15536 ) ;
#6340 = EDGE_CURVE ( 'NONE', #7837, #4507, #8067, .T. ) ;
#6341 = EDGE_CURVE ( 'NONE', #9965, #17590, #18167, .T. ) ;
#6342 = ADVANCED_FACE ( 'NONE', ( #9573 ), #11972, .T. ) ;
#6343 = EDGE_LOOP ( 'NONE', ( #1786, #9715, #1010, #8655, #5901, #8474, #15691, #13381, #7239, #18533, #2145, #3273, #10553, #11161, #4625, #10740, #296, #17379, #1754, #13240, #7044, #6903, #15472, #11839, #11143, #3021, #11539, #676, #3492, #17503, #3435, #6180, #17010, #17910, #14961, #13072, #17257, #9511, #12697, #17489, #1349, #15225, #1947, #5457, #7890, #10580, #2251, #4129, #3874, #11421, #7586, #13474, #8224, #2191, #7916, #4267, #6787, #13685, #9781, #8752, #4675, #11092, #16039, #18482 ) ) ;
#6344 =( NAMED_UNIT ( * ) SI_UNIT ( $, .STERADIAN. ) SOLID_ANGLE_UNIT ( ) );
#6345 = CARTESIAN_POINT ( 'NONE',  ( 1.847412631396506022, -10.09191835241968427, 7.278870946904215877 ) ) ;
#6346 = DIRECTION ( 'NONE',  ( 1.224646799147353207E-16, 1.000000000000000000, -0.000000000000000000 ) ) ;
#6348 = VERTEX_POINT ( 'NONE', #6808 ) ;
#6347 = CARTESIAN_POINT ( 'NONE',  ( 1.846138399168762101, 6.971848976711011225, 10.30487220521572667 ) ) ;
#6349 = CARTESIAN_POINT ( 'NONE',  ( 16.56872352241294521, 0.01027347319884441834, -0.001821578298044677175 ) ) ;
#6350 = ORIENTED_EDGE ( 'NONE', *, *, #6552, .F. ) ;
#6351 = LINE ( 'NONE', #14939, #6025 ) ;
#6352 = CARTESIAN_POINT ( 'NONE',  ( 1.861706995891668992, -11.66987142852987169, 4.359009869687201721 ) ) ;
#6353 = EDGE_CURVE ( 'NONE', #678, #16918, #4002, .T. ) ;
#6354 = EDGE_LOOP ( 'NONE', ( #14798, #12451, #1395, #11133 ) ) ;
#6355 = ORIENTED_EDGE ( 'NONE', *, *, #195, .T. ) ;
#6356 = CARTESIAN_POINT ( 'NONE',  ( 1.847034903785822690, -0.2299360331935046409, 12.44051878787773013 ) ) ;
#6357 = ORIENTED_EDGE ( 'NONE', *, *, #13275, .T. ) ;
#6358 = LINE ( 'NONE', #5001, #150 ) ;
#6359 = ORIENTED_EDGE ( 'NONE', *, *, #13742, .T. ) ;
#6360 =( NAMED_UNIT ( * ) SI_UNIT ( $, .STERADIAN. ) SOLID_ANGLE_UNIT ( ) );
#6361 =( NAMED_UNIT ( * ) PLANE_ANGLE_UNIT ( ) SI_UNIT ( $, .RADIAN. ) );
#6362 = CARTESIAN_POINT ( 'NONE',  ( 3.950837973638668288, 0.000000000000000000, 0.000000000000000000 ) ) ;
#6363 = CARTESIAN_POINT ( 'NONE',  ( 0.3307726912345197445, 13.74203354050372106, -0.5948952607473121379 ) ) ;
#6364 = CARTESIAN_POINT ( 'NONE',  ( 5.000000000000006217, -30.00000000000000000, 26.00000000000000000 ) ) ;
#6365 = VECTOR ( 'NONE', #3183, 1000.000000000000000 ) ;
#6366 = DIRECTION ( 'NONE',  ( 0.000000000000000000, 0.000000000000000000, -1.000000000000000000 ) ) ;
#6367 = DIRECTION ( 'NONE',  ( 0.000000000000000000, 0.000000000000000000, 1.000000000000000000 ) ) ;
#6368 = SURFACE_SIDE_STYLE ('',( #15241 ) ) ;
#6369 = CARTESIAN_POINT ( 'NONE',  ( 0.3058872367615226295, -4.821066432589418582, 12.87003593440626403 ) ) ;
#6370 = DIRECTION ( 'NONE',  ( 0.7635533937278214944, 0.5347026451755962917, -0.3620487483322465949 ) ) ;
#6371 = EDGE_CURVE ( 'NONE', #9140, #6750, #7891, .T. ) ;
#6372 = CARTESIAN_POINT ( 'NONE',  ( 2.750000000000000000, 0.000000000000000000, 0.000000000000000000 ) ) ;
#6373 = CARTESIAN_POINT ( 'NONE',  ( 18.30499999999999972, 0.000000000000000000, 0.000000000000000000 ) ) ;
#6374 = CARTESIAN_POINT ( 'NONE',  ( 0.3170788640506441158, 13.02120094575834131, -4.392045232375677344 ) ) ;
#6375 = DIRECTION ( 'NONE',  ( -0.7561779333270775005, -0.5081796452863273084, 0.4122479608995688327 ) ) ;
#6376 = VERTEX_POINT ( 'NONE', #615 ) ;
#6377 = ADVANCED_FACE ( 'NONE', ( #6439 ), #9784, .F. ) ;
#6378 = VERTEX_POINT ( 'NONE', #5367 ) ;
#6379 = ORIENTED_EDGE ( 'NONE', *, *, #2505, .F. ) ;
#6380 = ORIENTED_EDGE ( 'NONE', *, *, #11319, .T. ) ;
#6381 = CARTESIAN_POINT ( 'NONE',  ( 0.4754618798421162973, 10.80499583390525586, -8.775436892860994931 ) ) ;
#6382 = CARTESIAN_POINT ( 'NONE',  ( 0.3058872367615226295, -12.87003593440624982, -4.821066432589462103 ) ) ;
#6383 = FACE_OUTER_BOUND ( 'NONE', #12085, .T. ) ;
#6384 = DIRECTION ( 'NONE',  ( -1.000000000000000000, -0.000000000000000000, -0.000000000000000000 ) ) ;
#6385 = PRODUCT_DEFINITION_CONTEXT ( 'detailed design', #13881, 'design' ) ;
#6386 = CARTESIAN_POINT ( 'NONE',  ( 1.846138399168762989, 10.30487220521570357, 6.971848976711047641 ) ) ;
#6387 = CARTESIAN_POINT ( 'NONE',  ( 3.950837973638676281, -6.316429227969562632, 13.10350451991838128 ) ) ;
#6388 = LINE ( 'NONE', #14010, #3831 ) ;
#6389 = CARTESIAN_POINT ( 'NONE',  ( 0.3307726912345200776, 12.88561780039865745, -4.812300915532842005 ) ) ;
#6390 = CARTESIAN_POINT ( 'NONE',  ( 2.002547531651519996, 7.942910686618173344, 9.778737580845726640 ) ) ;
#6391 = CARTESIAN_POINT ( 'NONE',  ( 2.747332970342022840, -16.12459247543628393, 2.705255688517782975 ) ) ;
#6392 = ORIENTED_EDGE ( 'NONE', *, *, #1020, .T. ) ;
#6393 = EDGE_CURVE ( 'NONE', #1012, #3873, #13590, .T. ) ;
#6394 = VERTEX_POINT ( 'NONE', #13000 ) ;
#6395 = VERTEX_POINT ( 'NONE', #1345 ) ;
#6396 = ORIENTED_EDGE ( 'NONE', *, *, #15010, .F. ) ;
#6397 = DIRECTION ( 'NONE',  ( 0.7635533937278216055, 0.3620487483322444855, 0.5347026451755978460 ) ) ;
#6398 = EDGE_CURVE ( 'NONE', #18880, #11465, #2867, .T. ) ;
#6399 = PLANE ( 'NONE',  #7166 ) ;
#6400 = CARTESIAN_POINT ( 'NONE',  ( 3.950837973638675393, -2.591948120961706792, -14.31366178983255466 ) ) ;
#6401 = CARTESIAN_POINT ( 'NONE',  ( 3.353306896162455697, -5.573563251762193360, 12.78841260990236428 ) ) ;
#6402 = AXIS2_PLACEMENT_3D ( 'NONE', #14613, #1529, #4684 ) ;
#6403 = CARTESIAN_POINT ( 'NONE',  ( 8.438534575730034959, 4.221456476902665678, 5.415535776177536675 ) ) ;
#6404 = ORIENTED_EDGE ( 'NONE', *, *, #5521, .T. ) ;
#6405 = AXIS2_PLACEMENT_3D ( 'NONE', #7679, #17711, #14922 ) ;
#6406 = CARTESIAN_POINT ( 'NONE',  ( 1.847247051441598176, -4.004229874809106526, 11.78111530882021185 ) ) ;
#6407 = CARTESIAN_POINT ( 'NONE',  ( 0.3137051932979792457, 12.91601973349270871, 4.679953077377533965 ) ) ;
#6408 = CARTESIAN_POINT ( 'NONE',  ( -5.704021078596165140, 7.500000000000000000, -12.80826310103332943 ) ) ;
#6409 = CARTESIAN_POINT ( 'NONE',  ( -66.35602477868047799, 9.999999999999973355, 3.000000000000000000 ) ) ;
#6410 =( BOUNDED_SURFACE ( )  B_SPLINE_SURFACE ( 3, 1, ( 
 ( #948, #13852 ),
 ( #6604, #2459 ),
 ( #1033, #12428 ),
 ( #11280, #12788 ) ),
 .UNSPECIFIED., .F., .F., .T. ) 
 B_SPLINE_SURFACE_WITH_KNOTS ( ( 4, 4 ),
 ( 2, 2 ),
 ( 0.000000000000000000, 1.000000000000000000 ),
 ( 0.000000000000000000, 1.000000000000000000 ),
 .UNSPECIFIED. ) 
 GEOMETRIC_REPRESENTATION_ITEM ( )  RATIONAL_B_SPLINE_SURFACE ( (
 ( 1.000000000000000000, 1.000000000000000000),
 ( 0.7792777138730160313, 0.9689936506012927220),
 ( 0.7792777138730160313, 0.9689936506012927220),
 ( 1.000000000000000000, 1.000000000000000000) ) ) 
 REPRESENTATION_ITEM ( '' )  SURFACE ( )  );
#6411 = VECTOR ( 'NONE', #1864, 1000.000000000000227 ) ;
#6412 = DIRECTION ( 'NONE',  ( 0.000000000000000000, -1.000000000000000000, 0.000000000000000000 ) ) ;
#6413 = CARTESIAN_POINT ( 'NONE',  ( 2.636624412714237309, 15.80357026013209953, 2.862162146984226663 ) ) ;
#6414 = CARTESIAN_POINT ( 'NONE',  ( 2.002547531651519996, -7.942910686618100513, -9.778737580845787036 ) ) ;
#6415 = VERTEX_POINT ( 'NONE', #17117 ) ;
#6416 = CARTESIAN_POINT ( 'NONE',  ( 0.8740764193767259771, -13.31469591265765118, -5.211550415969147920 ) ) ;
#6418 = ORIENTED_EDGE ( 'NONE', *, *, #109, .T. ) ;
#6417 = CARTESIAN_POINT ( 'NONE',  ( 1.977228804422745512, -10.21522664410476366, -11.52787183731191512 ) ) ;
#6419 = PLANE ( 'NONE',  #16701 ) ;
#6420 = EDGE_CURVE ( 'NONE', #1319, #2485, #18075, .T. ) ;
#6421 = B_SPLINE_CURVE_WITH_KNOTS ( 'NONE', 3,
 ( #12558, #13722, #9423, #4842, #15248, #725 ),
 .UNSPECIFIED., .F., .F.,
 ( 4, 2, 4 ),
 ( 1.951563910473907981E-18, 0.0002017457492448081235, 0.0004034914984896142954 ),
 .UNSPECIFIED. ) ;
#6422 = EDGE_CURVE ( 'NONE', #15496, #5049, #7232, .T. ) ;
#6423 = ORIENTED_EDGE ( 'NONE', *, *, #15997, .F. ) ;
#6424 = CARTESIAN_POINT ( 'NONE',  ( 3.950837973638668288, 0.000000000000000000, 0.000000000000000000 ) ) ;
#6425 = CARTESIAN_POINT ( 'NONE',  ( 0.3753471441347580040, -7.499999999999771738, -13.03644311608535133 ) ) ;
#6426 = VERTEX_POINT ( 'NONE', #2576 ) ;
#6427 = CARTESIAN_POINT ( 'NONE',  ( 3.950837973638676281, -12.81214529934970336, -6.888253895133431115 ) ) ;
#6428 = CARTESIAN_POINT ( 'NONE',  ( 16.56753206892534891, -0.008432171035096412345, -0.004368917149004214288 ) ) ;
#6429 = DIRECTION ( 'NONE',  ( 1.000000000000000000, 0.000000000000000000, 0.000000000000000000 ) ) ;
#6430 = LINE ( 'NONE', #12341, #3515 ) ;
#6431 = ORIENTED_EDGE ( 'NONE', *, *, #9764, .T. ) ;
#6432 =( LENGTH_UNIT ( ) NAMED_UNIT ( * ) SI_UNIT ( .MILLI., .METRE. ) );
#6433 = CYLINDRICAL_SURFACE ( 'NONE', #358, 5.000000000000000888 ) ;
#6435 = VERTEX_POINT ( 'NONE', #8338 ) ;
#6434 = DIRECTION ( 'NONE',  ( -0.000000000000000000, -1.000000000000000000, -0.000000000000000000 ) ) ;
#6436 = CARTESIAN_POINT ( 'NONE',  ( 0.4754618798421162973, 10.80499583390512974, 8.775436892861156579 ) ) ;
#6437 = SHAPE_REPRESENTATION ( 'socket button head screw_iso_ISO 7380 - M5 x 20 - 20C', ( #2030 ), #809 ) ;
#6438 = ORIENTED_EDGE ( 'NONE', *, *, #14874, .F. ) ;
#6439 = FACE_OUTER_BOUND ( 'NONE', #4275, .T. ) ;
#6440 =( BOUNDED_SURFACE ( )  B_SPLINE_SURFACE ( 3, 1, ( 
 ( #5605, #18704 ),
 ( #11024, #3744 ),
 ( #13972, #12531 ),
 ( #3464, #9298 ) ),
 .UNSPECIFIED., .F., .F., .T. ) 
 B_SPLINE_SURFACE_WITH_KNOTS ( ( 4, 4 ),
 ( 2, 2 ),
 ( 0.000000000000000000, 1.000000000000000000 ),
 ( 0.000000000000000000, 1.000000000000000000 ),
 .UNSPECIFIED. ) 
 GEOMETRIC_REPRESENTATION_ITEM ( )  RATIONAL_B_SPLINE_SURFACE ( (
 ( 1.000000000000000000, 1.000000000000000000),
 ( 0.9933953342250436691, 0.8357391271907733676),
 ( 0.9933953342250436691, 0.8357391271907733676),
 ( 1.000000000000000000, 1.000000000000000000) ) ) 
 REPRESENTATION_ITEM ( '' )  SURFACE ( )  );
#6441 = CARTESIAN_POINT ( 'NONE',  ( -26.00000000000001066, -12.50000000000000178, 6.500000000000000888 ) ) ;
#6442 = ORIENTED_EDGE ( 'NONE', *, *, #5211, .T. ) ;
#6443 = EDGE_CURVE ( 'NONE', #7450, #9014, #18835, .T. ) ;
#6444 = EDGE_CURVE ( 'NONE', #799, #16688, #16582, .T. ) ;
#6445 = ORIENTED_EDGE ( 'NONE', *, *, #9378, .T. ) ;
#6446 = CARTESIAN_POINT ( 'NONE',  ( 0.3137051932979792457, 12.91601973349270871, 4.679953077377533965 ) ) ;
#6447 = ORIENTED_EDGE ( 'NONE', *, *, #9553, .T. ) ;
#6448 = CARTESIAN_POINT ( 'NONE',  ( 3.950837973638668288, 0.000000000000000000, 0.000000000000000000 ) ) ;
#6449 = ORIENTED_EDGE ( 'NONE', *, *, #9481, .T. ) ;
#6450 = SURFACE_SIDE_STYLE ('',( #12363 ) ) ;
#6451 = CARTESIAN_POINT ( 'NONE',  ( 16.56753206892534891, 0.004253784598196176658, -0.008490833999798941267 ) ) ;
#6452 = CARTESIAN_POINT ( 'NONE',  ( 1.846138399168762101, 12.43476674860266584, 0.4167076046095977149 ) ) ;
#6453 = DIRECTION ( 'NONE',  ( -1.000000000000000000, 0.000000000000000000, -0.000000000000000000 ) ) ;
#6454 = CARTESIAN_POINT ( 'NONE',  ( 3.950837973638668288, 0.000000000000000000, 0.000000000000000000 ) ) ;
#6455 = CARTESIAN_POINT ( 'NONE',  ( 8.522092701127531811, 5.397361180353207111, -4.388629235579518451 ) ) ;
#6456 = CARTESIAN_POINT ( 'NONE',  ( 2.636624412716913390, 14.14563173255587536, -7.605649742760633991 ) ) ;
#6457 = B_SPLINE_CURVE_WITH_KNOTS ( 'NONE', 3,
 ( #7542, #1696, #16027, #14885, #6101, #11924 ),
 .UNSPECIFIED., .F., .F.,
 ( 4, 2, 4 ),
 ( 0.000000000000000000, 0.001656992708822828484, 0.003313985417645657836 ),
 .UNSPECIFIED. ) ;
#6458 = CARTESIAN_POINT ( 'NONE',  ( 0.3151926232592457966, 8.137833541809381899, 11.07013665200797625 ) ) ;
#6459 = CARTESIAN_POINT ( 'NONE',  ( 2.353870697619111052, 12.05847592522643907, 4.720869121224175124 ) ) ;
#6460 = VECTOR ( 'NONE', #14318, 1000.000000000000000 ) ;
#6461 = CARTESIAN_POINT ( 'NONE',  ( -59.99999999999997158, -10.00000000000000888, 6.000000000000000000 ) ) ;
#6462 = CARTESIAN_POINT ( 'NONE',  ( 16.56679352167444819, 0.001390132774594440108, -0.009190982326619726375 ) ) ;
#6463 = B_SPLINE_CURVE_WITH_KNOTS ( 'NONE', 3,
 ( #9606, #12477, #5027, #13909, #4943, #18126, #823, #10968, #6664, #10774, #3501, #15342, #5125, #3778, #13733, #5303, #16788, #15258, #16875, #3687, #10878, #9518, #12566, #2253, #18309, #5216, #11057, #2431, #15437, #8190, #14007, #915, #9341, #6755, #18219, #9703, #16696, #2086 ),
 .UNSPECIFIED., .F., .F.,
 ( 4, 2, 2, 2, 2, 2, 2, 2, 2, 2, 2, 2, 2, 2, 2, 2, 2, 2, 4 ),
 ( 0.000000000000000000, 0.0009058109605214382685, 0.001811621921042876537, 0.002717432881564314697, 0.003623243842085754375, 0.004529054802607194487, 0.005434865763128634598, 0.006340676723650073843, 0.006793582203910795633, 0.007246487684171517424, 0.007699393164432237480, 0.008152298644692957535, 0.009058109605214399382, 0.009963920565735841228, 0.01086973152625728307, 0.01177554248677872319, 0.01268135344730016677, 0.01358716440782160688, 0.01449297536834305046 ),
 .UNSPECIFIED. ) ;
#6464 = ORIENTED_EDGE ( 'NONE', *, *, #13463, .F. ) ;
#6465 = EDGE_CURVE ( 'NONE', #5896, #7194, #15585, .T. ) ;
#6466 = ADVANCED_FACE ( 'NONE', ( #8519 ), #18553, .T. ) ;
#6467 = ADVANCED_FACE ( 'NONE', ( #7090 ), #12908, .F. ) ;
#6468 = ORIENTED_EDGE ( 'NONE', *, *, #16293, .F. ) ;
#6469 = ORIENTED_EDGE ( 'NONE', *, *, #56, .T. ) ;
#6470 = EDGE_LOOP ( 'NONE', ( #4005, #8505, #8800, #9232 ) ) ;
#6471 = ORIENTED_EDGE ( 'NONE', *, *, #18338, .F. ) ;
#6472 = CARTESIAN_POINT ( 'NONE',  ( 0.3151930723728406103, 11.07033375389132246, 8.137566970826403789 ) ) ;
#6473 = CARTESIAN_POINT ( 'NONE',  ( 0.4862570985993235340, 5.003653737315670647, -12.97920246947874112 ) ) ;
#6474 = PLANE ( 'NONE',  #17836 ) ;
#6475 = CARTESIAN_POINT ( 'NONE',  ( 2.636624412716062960, 2.862162146982868194, -15.80357026013419564 ) ) ;
#6476 = DIRECTION ( 'NONE',  ( -1.000000000000000000, 0.000000000000000000, 0.000000000000000000 ) ) ;
#6477 = CYLINDRICAL_SURFACE ( 'NONE', #9623, 2.499999999999999556 ) ;
#6478 = CARTESIAN_POINT ( 'NONE',  ( 3.950837973638668288, 0.000000000000000000, 0.000000000000000000 ) ) ;
#6479 = FACE_OUTER_BOUND ( 'NONE', #10978, .T. ) ;
#6480 = AXIS2_PLACEMENT_3D ( 'NONE', #1248, #12813, #15964 ) ;
#6481 = DIRECTION ( 'NONE',  ( -0.7561779333270775005, 0.5081796452863305280, -0.4122479608995649469 ) ) ;
#6482 = VERTEX_POINT ( 'NONE', #18453 ) ;
#6483 = PRODUCT_DEFINITION_SHAPE ( 'NONE', 'NONE',  #2073 ) ;
#6484 = ORIENTED_EDGE ( 'NONE', *, *, #9822, .T. ) ;
#6485 = ORIENTED_EDGE ( 'NONE', *, *, #509, .T. ) ;
#6486 = B_SPLINE_CURVE_WITH_KNOTS ( 'NONE', 3,
 ( #17600, #1542, #4512, #14534 ),
 .UNSPECIFIED., .F., .F.,
 ( 4, 4 ),
 ( 0.000000000000000000, 0.002004993803842769744 ),
 .UNSPECIFIED. ) ;
#6487 = ORIENTED_EDGE ( 'NONE', *, *, #14431, .F. ) ;
#6488 = CARTESIAN_POINT ( 'NONE',  ( 1.846138399168762101, -7.646096044339961040, 9.815003036200383946 ) ) ;
#6489 = EDGE_CURVE ( 'NONE', #4587, #5607, #9756, .T. ) ;
#6490 = CARTESIAN_POINT ( 'NONE',  ( 16.57778382496167424, 0.01306626476309289374, -0.007244066302946823403 ) ) ;
#6491 = EDGE_CURVE ( 'NONE', #1036, #4171, #1581, .T. ) ;
#6492 = DIRECTION ( 'NONE',  ( -1.000000000000000000, 0.000000000000000000, 0.000000000000000000 ) ) ;
#6493 = CARTESIAN_POINT ( 'NONE',  ( 8.522092701127531811, 6.722964936702122252, -1.786985377231962380 ) ) ;
#6494 = AXIS2_PLACEMENT_3D ( 'NONE', #17822, #9122, #8918 ) ;
#6495 = B_SPLINE_CURVE_WITH_KNOTS ( 'NONE', 3,
 ( #17740, #16863, #3768, #9225, #1874, #9326, #5202, #7810, #13803, #15154, #6269, #2239, #10861 ),
 .UNSPECIFIED., .F., .F.,
 ( 4, 3, 3, 3, 4 ),
 ( 0.000000000000000000, 0.0002299804304191490972, 0.0004599608082120256055, 0.0006467586077648033180, 0.0008336169836825999165 ),
 .UNSPECIFIED. ) ;
#6496 = DIRECTION ( 'NONE',  ( 0.000000000000000000, 0.000000000000000000, -1.000000000000000000 ) ) ;
#6497 = ORIENTED_EDGE ( 'NONE', *, *, #11876, .F. ) ;
#6498 = CARTESIAN_POINT ( 'NONE',  ( 1.977228804421385933, 15.33060379559031539, -1.488378900181928532 ) ) ;
#6499 = CARTESIAN_POINT ( 'NONE',  ( 1.861706995891675653, 0.5394761475745838419, 12.44571539481144207 ) ) ;
#6500 = CARTESIAN_POINT ( 'NONE',  ( 0.06860918897775840353, 7.499999999999997335, -13.03178490627139219 ) ) ;
#6501 = CARTESIAN_POINT ( 'NONE',  ( 1.560000000000000053, -1.299038105676658450, -0.7500000000000007772 ) ) ;
#6502 = DIRECTION ( 'NONE',  ( -0.7071067811865486830, 8.659560562354921765E-17, -0.7071067811865464625 ) ) ;
#6503 = CARTESIAN_POINT ( 'NONE',  ( 3.950837973638676281, -1.958075594453890789, 14.41405733518059940 ) ) ;
#6504 = CARTESIAN_POINT ( 'NONE',  ( 0.8740764193768816304, 0.8420116711623857331, -14.27348595579795010 ) ) ;
#6505 = VERTEX_POINT ( 'NONE', #16461 ) ;
#6506 = EDGE_CURVE ( 'NONE', #17181, #8687, #15636, .T. ) ;
#6508 = ORIENTED_EDGE ( 'NONE', *, *, #13275, .F. ) ;
#6507 = CARTESIAN_POINT ( 'NONE',  ( 1.847380140988738484, 11.79969976631077699, -3.949801494731646656 ) ) ;
#6509 = CARTESIAN_POINT ( 'NONE',  ( 0.000000000000000000, 0.000000000000000000, 0.000000000000000000 ) ) ;
#6510 = PRODUCT_DEFINITION ( 'UNKNOWN', '', #9585, #6385 ) ;
#6511 = ADVANCED_FACE ( 'NONE', ( #3144 ), #10651, .F. ) ;
#6512 = ADVANCED_FACE ( 'NONE', ( #1931 ), #11756, .F. ) ;
#6513 = AXIS2_PLACEMENT_3D ( 'NONE', #1773, #1669, #15910 ) ;
#6514 = ORIENTED_EDGE ( 'NONE', *, *, #17078, .F. ) ;
#6515 = CARTESIAN_POINT ( 'NONE',  ( 16.56872352241294521, -0.001442253899401880124, -0.01033355228142401362 ) ) ;
#6516 = EDGE_CURVE ( 'NONE', #15230, #4268, #5534, .T. ) ;
#6517 = CARTESIAN_POINT ( 'NONE',  ( -0.5119965487699434936, -7.500000000000230926, -13.04039602617929638 ) ) ;
#6518 =( BOUNDED_SURFACE ( )  B_SPLINE_SURFACE ( 3, 1, ( 
 ( #7467, #11479 ),
 ( #2757, #17298 ),
 ( #17488, #14711 ),
 ( #15957, #13281 ) ),
 .UNSPECIFIED., .F., .F., .T. ) 
 B_SPLINE_SURFACE_WITH_KNOTS ( ( 4, 4 ),
 ( 2, 2 ),
 ( 0.000000000000000000, 1.000000000000000000 ),
 ( 0.000000000000000000, 1.000000000000000000 ),
 .UNSPECIFIED. ) 
 GEOMETRIC_REPRESENTATION_ITEM ( )  RATIONAL_B_SPLINE_SURFACE ( (
 ( 1.000000000000000000, 1.000000000000000000),
 ( 0.9593108457356467333, 0.9995965569486454649),
 ( 0.9593108457356467333, 0.9995965569486454649),
 ( 1.000000000000000000, 1.000000000000000000) ) ) 
 REPRESENTATION_ITEM ( '' )  SURFACE ( )  );
#6519 = ORIENTED_EDGE ( 'NONE', *, *, #18386, .F. ) ;
#6520 = CARTESIAN_POINT ( 'NONE',  ( 3.950837973638676281, 10.05648675950141602, -10.51028938476206953 ) ) ;
#6521 = CARTESIAN_POINT ( 'NONE',  ( 3.512766787570769100, 13.55823433651956833, -6.535475144496838418 ) ) ;
#6522 = CARTESIAN_POINT ( 'NONE',  ( 2.636624412714236865, 0.000000000000000000, 0.000000000000000000 ) ) ;
#6523 = CARTESIAN_POINT ( 'NONE',  ( 3.686287386450715076E-15, -28.26180729995786933, 25.01316734529526187 ) ) ;
#6524 = CONICAL_SURFACE ( 'NONE', #11108, 14.54644660717763927, 0.8559913436420816257 ) ;
#6525 = EDGE_CURVE ( 'NONE', #16455, #1566, #1909, .T. ) ;
#6526 = SURFACE_SIDE_STYLE ('',( #12169 ) ) ;
#6527 = VECTOR ( 'NONE', #3944, 1000.000000000000000 ) ;
#6528 = CARTESIAN_POINT ( 'NONE',  ( 16.58200780006414732, -0.01041078477704051979, -0.004047297414159007484 ) ) ;
#6529 = CARTESIAN_POINT ( 'NONE',  ( -199.9999999999999716, -25.00000000000003197, 0.000000000000000000 ) ) ;
#6531 = ORIENTED_EDGE ( 'NONE', *, *, #8329, .F. ) ;
#6530 = FACE_OUTER_BOUND ( 'NONE', #12920, .T. ) ;
#6532 = CARTESIAN_POINT ( 'NONE',  ( 16.57778382496167424, 0.007244066302947695102, -0.01306626476309380794 ) ) ;
#6533 = EDGE_CURVE ( 'NONE', #13259, #17499, #16363, .T. ) ;
#6534 = ORIENTED_EDGE ( 'NONE', *, *, #513, .F. ) ;
#6535 = CARTESIAN_POINT ( 'NONE',  ( 0.3137051932979757485, 8.442169467526850823, 10.83767969834806166 ) ) ;
#6536 = CARTESIAN_POINT ( 'NONE',  ( 3.950837973638675393, -13.10350451991845055, 6.316429227969417859 ) ) ;
#6537 = ORIENTED_EDGE ( 'NONE', *, *, #7881, .F. ) ;
#6538 = ORIENTED_EDGE ( 'NONE', *, *, #17902, .T. ) ;
#6539 = DIRECTION ( 'NONE',  ( 0.000000000000000000, 0.000000000000000000, 1.000000000000000000 ) ) ;
#6540 = PLANE ( 'NONE',  #3506 ) ;
#6541 = VERTEX_POINT ( 'NONE', #108 ) ;
#6542 = FILL_AREA_STYLE ('',( #10748 ) ) ;
#6543 = CARTESIAN_POINT ( 'NONE',  ( 3.686287386450715076E-15, -16.60000000000000142, 25.01316734529526187 ) ) ;
#6544 = VECTOR ( 'NONE', #3007, 1000.000000000000114 ) ;
#6545 = CIRCLE ( 'NONE', #16308, 3.999999999999993339 ) ;
#6546 = CARTESIAN_POINT ( 'NONE',  ( 0.3137051932979775248, 10.83767969834815581, -8.442169467526731808 ) ) ;
#6547 = CARTESIAN_POINT ( 'NONE',  ( 2.123976203522053741, 14.31368049382978569, -6.261444813538409981 ) ) ;
#6548 = CARTESIAN_POINT ( 'NONE',  ( 16.56782317627811096, 0.007739510688079516768, 0.006045301465876390737 ) ) ;
#6549 = SHAPE_DEFINITION_REPRESENTATION ( #10270, #8995 ) ;
#6550 = SHAPE_REPRESENTATION_RELATIONSHIP ( 'NONE' , 'NONE' ,  #11674, #5561 ) ;
#6551 = CARTESIAN_POINT ( 'NONE',  ( 1.959283090834841090, -10.53516775895155000, -6.829027319138364582 ) ) ;
#6552 = EDGE_CURVE ( 'NONE', #15452, #4150, #7580, .T. ) ;
#6553 = CARTESIAN_POINT ( 'NONE',  ( 0.8740764193769881008, 5.211550415969331773, -13.31469591265785901 ) ) ;
#6554 =( BOUNDED_SURFACE ( )  B_SPLINE_SURFACE ( 3, 1, ( 
 ( #1993, #7734 ),
 ( #16611, #12126 ),
 ( #17959, #15264 ),
 ( #4859, #16526 ) ),
 .UNSPECIFIED., .F., .F., .T. ) 
 B_SPLINE_SURFACE_WITH_KNOTS ( ( 4, 4 ),
 ( 2, 2 ),
 ( 0.000000000000000000, 1.000000000000000000 ),
 ( 0.000000000000000000, 1.000000000000000000 ),
 .UNSPECIFIED. ) 
 GEOMETRIC_REPRESENTATION_ITEM ( )  RATIONAL_B_SPLINE_SURFACE ( (
 ( 1.000000000000000000, 1.000000000000000000),
 ( 0.9593108457356467333, 0.9995965569486454649),
 ( 0.9593108457356467333, 0.9995965569486454649),
 ( 1.000000000000000000, 1.000000000000000000) ) ) 
 REPRESENTATION_ITEM ( '' )  SURFACE ( )  );
#6555 =( BOUNDED_SURFACE ( )  B_SPLINE_SURFACE ( 3, 1, ( 
 ( #9190, #7873 ),
 ( #9098, #7770 ),
 ( #13686, #12163 ),
 ( #7587, #17803 ) ),
 .UNSPECIFIED., .F., .F., .T. ) 
 B_SPLINE_SURFACE_WITH_KNOTS ( ( 4, 4 ),
 ( 2, 2 ),
 ( 0.000000000000000000, 1.000000000000000000 ),
 ( 0.000000000000000000, 1.000000000000000000 ),
 .UNSPECIFIED. ) 
 GEOMETRIC_REPRESENTATION_ITEM ( )  RATIONAL_B_SPLINE_SURFACE ( (
 ( 1.000000000000000000, 1.000000000000000000),
 ( 0.7792777138730158093, 0.9689936506012928330),
 ( 0.7792777138730158093, 0.9689936506012928330),
 ( 1.000000000000000000, 1.000000000000000000) ) ) 
 REPRESENTATION_ITEM ( '' )  SURFACE ( )  );
#6556 = FACE_OUTER_BOUND ( 'NONE', #1688, .T. ) ;
#6557 = CARTESIAN_POINT ( 'NONE',  ( -110.4113270445337918, -81.60345299795268659, -91.28051051278382033 ) ) ;
#6558 = AXIS2_PLACEMENT_3D ( 'NONE', #3362, #10254, #16086 ) ;
#6559 = DIRECTION ( 'NONE',  ( -1.239088197126290570E-16, 1.000000000000000000, 0.000000000000000000 ) ) ;
#6560 = ORIENTED_EDGE ( 'NONE', *, *, #4238, .F. ) ;
#6561 = ORIENTED_EDGE ( 'NONE', *, *, #12750, .T. ) ;
#6562 = EDGE_LOOP ( 'NONE', ( #11555, #2649, #18485, #6318 ) ) ;
#6563 = ORIENTED_EDGE ( 'NONE', *, *, #6065, .T. ) ;
#6564 = CYLINDRICAL_SURFACE ( 'NONE', #4777, 5.000000000000000000 ) ;
#6565 = DIRECTION ( 'NONE',  ( -0.000000000000000000, 0.000000000000000000, 1.000000000000000000 ) ) ;
#6566 = CARTESIAN_POINT ( 'NONE',  ( 1.254255976357841584, 1.011593778944668731, -14.64488542023482331 ) ) ;
#6567 = CARTESIAN_POINT ( 'NONE',  ( -59.99999999999997158, -10.00000000000000888, 6.000000000000000000 ) ) ;
#6568 = CIRCLE ( 'NONE', #17233, 16.06066017081991149 ) ;
#6569 = VECTOR ( 'NONE', #478, 1000.000000000000000 ) ;
#6570 = EDGE_CURVE ( 'NONE', #204, #14839, #14091, .T. ) ;
#6571 = CARTESIAN_POINT ( 'NONE',  ( 0.3137051932979757485, 12.91601973349276733, -4.679953077377353665 ) ) ;
#6572 = EDGE_CURVE ( 'NONE', #4080, #12131, #4402, .T. ) ;
#6573 = CARTESIAN_POINT ( 'NONE',  ( -194.9999999999999716, -10.00000000000003020, 11.00000000000000000 ) ) ;
#6574 = EDGE_CURVE ( 'NONE', #3683, #15961, #395, .T. ) ;
#6575 = LINE ( 'NONE', #9247, #241 ) ;
#6576 = DIRECTION ( 'NONE',  ( 0.000000000000000000, 0.000000000000000000, 1.000000000000000000 ) ) ;
#6577 = B_SPLINE_CURVE_WITH_KNOTS ( 'NONE', 3,
 ( #9656, #2560, #13959, #870, #5258, #6711 ),
 .UNSPECIFIED., .F., .F.,
 ( 4, 2, 4 ),
 ( 2.622335209753013447E-18, 0.0002017457492448088824, 0.0004034914984896151085 ),
 .UNSPECIFIED. ) ;
#6578 = DIRECTION ( 'NONE',  ( 1.000000000000000000, 0.000000000000000000, 0.000000000000000000 ) ) ;
#6579 = ORIENTED_EDGE ( 'NONE', *, *, #18312, .F. ) ;
#6580 = ORIENTED_EDGE ( 'NONE', *, *, #16070, .F. ) ;
#6581 = EDGE_LOOP ( 'NONE', ( #158, #3068, #15724, #16261 ) ) ;
#6582 = AXIS2_PLACEMENT_3D ( 'NONE', #3355, #13300, #13203 ) ;
#6583 = ORIENTED_EDGE ( 'NONE', *, *, #12462, .F. ) ;
#6584 = DIRECTION ( 'NONE',  ( 0.000000000000000000, 0.000000000000000000, -1.000000000000000000 ) ) ;
#6585 = CARTESIAN_POINT ( 'NONE',  ( 2.123976203522053741, 10.37815841598491851, 11.67822624909929452 ) ) ;
#6586 = LINE ( 'NONE', #7747, #11140 ) ;
#6587 = CARTESIAN_POINT ( 'NONE',  ( 2.636624412716045196, 11.10302021257998994, -11.60464335004042447 ) ) ;
#6588 = FACE_OUTER_BOUND ( 'NONE', #6729, .T. ) ;
#6589 = ORIENTED_EDGE ( 'NONE', *, *, #14493, .F. ) ;
#6590 = CARTESIAN_POINT ( 'NONE',  ( 0.3137051932979792457, 11.37800749014131263, 7.698472063774513430 ) ) ;
#6591 = CARTESIAN_POINT ( 'NONE',  ( 1.562796894703937678, 4.769696007084728073, -1.500000000000000000 ) ) ;
#6592 = CARTESIAN_POINT ( 'NONE',  ( 0.1127451301831694647, 7.499999999999999112, -14.18240585847532742 ) ) ;
#6593 = CARTESIAN_POINT ( 'NONE',  ( -30.00000000000000355, -12.50000000000000178, 6.500000000000000888 ) ) ;
#6594 = CARTESIAN_POINT ( 'NONE',  ( 0.4754618798421162973, 3.583352865732857495, -13.45049478164055756 ) ) ;
#6595 = CARTESIAN_POINT ( 'NONE',  ( 3.950837973638675393, -6.888253895133384930, 12.81214529934972823 ) ) ;
#6596 = DIRECTION ( 'NONE',  ( 0.000000000000000000, 0.000000000000000000, 1.000000000000000000 ) ) ;
#6597 = AXIS2_PLACEMENT_3D ( 'NONE', #8691, #11660, #17485 ) ;
#6598 = STYLED_ITEM ( 'NONE', ( #4444 ), #18114 ) ;
#6599 = CARTESIAN_POINT ( 'NONE',  ( 1.977436885026506497, -3.321781585408274839, -15.04044112860335147 ) ) ;
#6600 = VERTEX_POINT ( 'NONE', #13480 ) ;
#6601 = EDGE_CURVE ( 'NONE', #11517, #13667, #5839, .T. ) ;
#6603 = ORIENTED_EDGE ( 'NONE', *, *, #5540, .F. ) ;
#6602 = CARTESIAN_POINT ( 'NONE',  ( 16.56872352241294521, 0.01027347319884366721, 0.001821578298043820656 ) ) ;
#6604 = CARTESIAN_POINT ( 'NONE',  ( 16.57210152137263393, 0.008007331252333427934, -0.01214401161737626612 ) ) ;
#6605 = ADVANCED_FACE ( 'NONE', ( #10428 ), #12579, .F. ) ;
#6606 = ORIENTED_EDGE ( 'NONE', *, *, #3410, .F. ) ;
#6607 = DIRECTION ( 'NONE',  ( -1.000000000000000000, -0.000000000000000000, -0.000000000000000000 ) ) ;
#6608 = VECTOR ( 'NONE', #7632, 1000.000000000000000 ) ;
#6609 = EDGE_LOOP ( 'NONE', ( #5674, #5249, #155, #17840 ) ) ;
#6610 = CARTESIAN_POINT ( 'NONE',  ( -5.045697689581268186, -7.500000000000132339, -13.04808138403488549 ) ) ;
#6611 = VERTEX_POINT ( 'NONE', #16553 ) ;
#6612 = CARTESIAN_POINT ( 'NONE',  ( 25.00000000000000000, -2.500000000000000444, -12.00000000000000000 ) ) ;
#6613 = B_SPLINE_CURVE_WITH_KNOTS ( 'NONE', 3,
 ( #8724, #18751, #1079, #11598, #12646, #18570, #5650, #15696, #10062, #12830, #6826, #14550, #18657 ),
 .UNSPECIFIED., .F., .F.,
 ( 4, 3, 3, 3, 4 ),
 ( 1.734723475976807094E-18, 0.0002299804304191470643, 0.0004599608082120238165, 0.0006467586077648016917, 0.0008336169836825990491 ),
 .UNSPECIFIED. ) ;
#6614 = DIRECTION ( 'NONE',  ( 0.000000000000000000, 0.000000000000000000, 1.000000000000000000 ) ) ;
#6615 = CARTESIAN_POINT ( 'NONE',  ( 0.4862570985993252548, -5.003653737315580052, 12.97920246947877665 ) ) ;
#6616 = DIRECTION ( 'NONE',  ( 0.000000000000000000, 0.000000000000000000, -1.000000000000000000 ) ) ;
#6617 = EDGE_CURVE ( 'NONE', #8437, #16664, #1052, .T. ) ;
#6618 = COLOUR_RGB ( '', 0.31764706, 0.68627451, 0.89019608) ;
#6619 = DIRECTION ( 'NONE',  ( -5.782411586589358625E-16, 1.000000000000000000, 0.000000000000000000 ) ) ;
#6620 = EDGE_CURVE ( 'NONE', #1184, #17773, #17013, .T. ) ;
#6621 = ADVANCED_FACE ( 'NONE', ( #17098 ), #9554, .T. ) ;
#6622 = COLOUR_RGB ( '', 0.08235294, 0.09019608, 0.10196078) ;
#6623 = B_SPLINE_CURVE_WITH_KNOTS ( 'NONE', 3,
 ( #11018, #2305, #8150, #6717, #12526, #18360 ),
 .UNSPECIFIED., .F., .F.,
 ( 4, 2, 4 ),
 ( 1.939479807224432123E-18, 0.001657017934711440621, 0.003314035869422879074 ),
 .UNSPECIFIED. ) ;
#6624 = CARTESIAN_POINT ( 'NONE',  ( 16.56872352241294521, 0.007512283835804314455, -0.007240717549633915451 ) ) ;
#6626 = ORIENTED_EDGE ( 'NONE', *, *, #14384, .F. ) ;
#6625 = CARTESIAN_POINT ( 'NONE',  ( 0.3720661004400040439, -0.7231997263363842965, -13.79610186261031046 ) ) ;
#6627 = CARTESIAN_POINT ( 'NONE',  ( -4.999999999999995559, -27.00000000000000000, 26.00000000000000000 ) ) ;
#6628 = AXIS2_PLACEMENT_3D ( 'NONE', #14467, #5401, #1379 ) ;
#6629 = CARTESIAN_POINT ( 'NONE',  ( 16.58200780006414732, -0.009393638146078483672, -0.006043560077721808060 ) ) ;
#6630 = CARTESIAN_POINT ( 'NONE',  ( 1.959283090834841090, 11.71721539537261414, -4.509128209890848282 ) ) ;
#6631 = EDGE_CURVE ( 'NONE', #4268, #202, #8228, .T. ) ;
#6632 =( BOUNDED_SURFACE ( )  B_SPLINE_SURFACE ( 3, 1, ( 
 ( #2790, #7027 ),
 ( #11422, #4342 ),
 ( #7115, #18236 ),
 ( #9533, #7220 ) ),
 .UNSPECIFIED., .F., .F., .T. ) 
 B_SPLINE_SURFACE_WITH_KNOTS ( ( 4, 4 ),
 ( 2, 2 ),
 ( 0.000000000000000000, 1.000000000000000000 ),
 ( 0.000000000000000000, 1.000000000000000000 ),
 .UNSPECIFIED. ) 
 GEOMETRIC_REPRESENTATION_ITEM ( )  RATIONAL_B_SPLINE_SURFACE ( (
 ( 1.000000000000000000, 1.000000000000000000),
 ( 0.9933953342250436691, 0.8357391271907733676),
 ( 0.9933953342250436691, 0.8357391271907733676),
 ( 1.000000000000000000, 1.000000000000000000) ) ) 
 REPRESENTATION_ITEM ( '' )  SURFACE ( )  );
#6633 = ORIENTED_EDGE ( 'NONE', *, *, #11806, .F. ) ;
#6634 = ORIENTED_EDGE ( 'NONE', *, *, #8643, .F. ) ;
#6635 = CARTESIAN_POINT ( 'NONE',  ( 0.3137051932979792457, -0.4596302728640728752, 13.73004976592201842 ) ) ;
#6636 = AXIS2_PLACEMENT_3D ( 'NONE', #14126, #12696, #18527 ) ;
#6637 = CARTESIAN_POINT ( 'NONE',  ( 2.636624412714237309, 14.14563173255211126, 7.605649742762011556 ) ) ;
#6638 = EDGE_LOOP ( 'NONE', ( #13503, #17754, #10790, #17207 ) ) ;
#6639 = CIRCLE ( 'NONE', #7552, 1.000000000000000000 ) ;
#6640 = CARTESIAN_POINT ( 'NONE',  ( 0.3150686449036049219, 4.391272911157320991, 13.01866258978838609 ) ) ;
#6641 = EDGE_CURVE ( 'NONE', #14355, #14429, #16554, .T. ) ;
#6642 = FACE_OUTER_BOUND ( 'NONE', #16962, .T. ) ;
#6643 = CARTESIAN_POINT ( 'NONE',  ( -1.500000000000000000, -2.869946927167511679E-16, 7.000000000000000000 ) ) ;
#6644 = CARTESIAN_POINT ( 'NONE',  ( -112.7602355015299338, -81.60345299795268659, -92.39524324337544670 ) ) ;
#6645 = CARTESIAN_POINT ( 'NONE',  ( 16.57778382496167424, -0.002851818597093308278, -0.01466529584256674387 ) ) ;
#6646 = B_SPLINE_CURVE_WITH_KNOTS ( 'NONE', 3,
 ( #5198, #12828, #18655, #11044 ),
 .UNSPECIFIED., .F., .F.,
 ( 4, 4 ),
 ( 9.796581096179191873E-17, 0.002004993803842611885 ),
 .UNSPECIFIED. ) ;
#6647 = DIRECTION ( 'NONE',  ( -1.000000000000000000, -0.000000000000000000, -0.000000000000000000 ) ) ;
#6648 = APPLICATION_PROTOCOL_DEFINITION ( 'draft international standard', 'automotive_design', 1998, #12898 ) ;
#6649 =( NAMED_UNIT ( * ) SI_UNIT ( $, .STERADIAN. ) SOLID_ANGLE_UNIT ( ) );
#6650 = CARTESIAN_POINT ( 'NONE',  ( 16.57605080000000086, 0.000000000000000000, 5.000000000000000000 ) ) ;
#6651 = CARTESIAN_POINT ( 'NONE',  ( 2.636624412714292376, 11.60464335004048309, 11.10302021257707850 ) ) ;
#6652 = CARTESIAN_POINT ( 'NONE',  ( 16.56753206892534891, 0.001421777558676785977, 0.009389754735541558373 ) ) ;
#6653 = DIRECTION ( 'NONE',  ( -1.000000000000000000, -0.000000000000000000, -0.000000000000000000 ) ) ;
#6654 = CARTESIAN_POINT ( 'NONE',  ( 2.697797270744666243, -11.26906156738832188, 7.053988368581824986 ) ) ;
#6655 = CARTESIAN_POINT ( 'NONE',  ( 0.4754618798421171855, -11.68486377711960778, -7.564402563418600067 ) ) ;
#6656 = ORIENTED_EDGE ( 'NONE', *, *, #510, .T. ) ;
#6657 = ADVANCED_FACE ( 'NONE', ( #14046 ), #1035, .F. ) ;
#6658 = ORIENTED_EDGE ( 'NONE', *, *, #1474, .F. ) ;
#6659 = EDGE_LOOP ( 'NONE', ( #14671, #4196, #18164, #18040 ) ) ;
#6660 = B_SPLINE_CURVE_WITH_KNOTS ( 'NONE', 3,
 ( #7764, #17794, #679, #13572 ),
 .UNSPECIFIED., .F., .F.,
 ( 4, 4 ),
 ( 1.464275143509529362E-17, 0.003005512676784844427 ),
 .UNSPECIFIED. ) ;
#6661 = ORIENTED_EDGE ( 'NONE', *, *, #14022, .T. ) ;
#6662 = EDGE_CURVE ( 'NONE', #14073, #16368, #12275, .T. ) ;
#6663 = CARTESIAN_POINT ( 'NONE',  ( 0.3148208552358953138, 11.24855514421875569, 7.888357771040743316 ) ) ;
#6664 = CARTESIAN_POINT ( 'NONE',  ( 3.381675179273347265, -7.500000000000001776, -16.15172605159659369 ) ) ;
#6665 = CARTESIAN_POINT ( 'NONE',  ( 3.074695600507118431, 2.772091048739504959, -15.30693405987805811 ) ) ;
#6666 = FACE_OUTER_BOUND ( 'NONE', #18433, .T. ) ;
#6667 = CARTESIAN_POINT ( 'NONE',  ( 0.4385251269669978580, 10.76637725024251857, 8.732456510146114681 ) ) ;
#6668 = CARTESIAN_POINT ( 'NONE',  ( 0.3137051932979757485, 12.91601973349276733, -4.679953077377353665 ) ) ;
#6669 = CARTESIAN_POINT ( 'NONE',  ( 1.959212340397943120, -7.909199412631233272, 9.750290364083607386 ) ) ;
#6670 = CARTESIAN_POINT ( 'NONE',  ( 1.845756295923373758, 7.694561132136944259, 9.776763338604617104 ) ) ;
#6671 = CARTESIAN_POINT ( 'NONE',  ( 2.697797270744669351, 3.226410068829429711, 12.89731672021091846 ) ) ;
#6672 = CONICAL_SURFACE ( 'NONE', #17648, 14.54644660717763927, 0.8559913436420816257 ) ;
#6673 = ORIENTED_EDGE ( 'NONE', *, *, #9598, .T. ) ;
#6674 = VERTEX_POINT ( 'NONE', #4004 ) ;
#6675 = ORIENTED_EDGE ( 'NONE', *, *, #15896, .F. ) ;
#6676 = ORIENTED_EDGE ( 'NONE', *, *, #10308, .F. ) ;
#6677 = CARTESIAN_POINT ( 'NONE',  ( 2.636624412715093513, -14.14563173255330142, 7.605649742761597665 ) ) ;
#6678 = ADVANCED_FACE ( 'NONE', ( #6702 ), #14536, .F. ) ;
#6679 = ADVANCED_FACE ( 'NONE', ( #12601 ), #14424, .F. ) ;
#6680 = EDGE_CURVE ( 'NONE', #1784, #14201, #18390, .T. ) ;
#6681 = CARTESIAN_POINT ( 'NONE',  ( 2.697797270744668019, -0.9169917281808188658, 13.26309265156976913 ) ) ;
#6682 = DIRECTION ( 'NONE',  ( -1.000000000000000000, -0.000000000000000000, -0.000000000000000000 ) ) ;
#6683 = CARTESIAN_POINT ( 'NONE',  ( 16.56753206892534891, 0.008432171035096382855, 0.004368917149004273269 ) ) ;
#6684 = PLANE ( 'NONE',  #13921 ) ;
#6685 = ORIENTED_EDGE ( 'NONE', *, *, #2443, .T. ) ;
#6686 = CARTESIAN_POINT ( 'NONE',  ( 0.4754618798421167414, -10.80499583390506402, -8.775436892861231186 ) ) ;
#6687 = CARTESIAN_POINT ( 'NONE',  ( 1.959283090834855745, 0.6676170829052219258, 12.53713130127477982 ) ) ;
#6688 = CARTESIAN_POINT ( 'NONE',  ( -3.382406833283016390, 7.499999999999999112, -16.15212677409211040 ) ) ;
#6689 = CARTESIAN_POINT ( 'NONE',  ( 1.959212340397943120, -7.909199412631233272, 9.750290364083607386 ) ) ;
#6690 = CARTESIAN_POINT ( 'NONE',  ( 8.522092701127531811, 4.388629235579577070, 5.397361180353158261 ) ) ;
#6691 = DIRECTION ( 'NONE',  ( -1.000000000000000000, 0.000000000000000000, 0.000000000000000000 ) ) ;
#6692 = CARTESIAN_POINT ( 'NONE',  ( 3.074695600507159732, -15.30693405987801370, -2.772091048739451669 ) ) ;
#6693 = DIRECTION ( 'NONE',  ( 0.000000000000000000, 0.000000000000000000, 1.000000000000000000 ) ) ;
#6694 = ORIENTED_EDGE ( 'NONE', *, *, #16781, .T. ) ;
#6695 = APPLICATION_CONTEXT ( 'automotive_design' ) ;
#6697 = ORIENTED_EDGE ( 'NONE', *, *, #18691, .T. ) ;
#6696 = CARTESIAN_POINT ( 'NONE',  ( 1.846955891736114852, 11.74973605926570386, -4.094751675596581819 ) ) ;
#6698 = DIRECTION ( 'NONE',  ( -0.000000000000000000, -0.000000000000000000, 1.000000000000000000 ) ) ;
#6699 = CIRCLE ( 'NONE', #12483, 2.500000000000000000 ) ;
#6700 = B_SPLINE_CURVE_WITH_KNOTS ( 'NONE', 3,
 ( #9049, #17951, #10483, #12015, #1792, #13439 ),
 .UNSPECIFIED., .F., .F.,
 ( 4, 2, 4 ),
 ( 4.206917491929696500E-17, 0.0002014099069817281611, 0.0004028198139634142552 ),
 .UNSPECIFIED. ) ;
#6701 = ADVANCED_FACE ( 'NONE', ( #8137 ), #863, .T. ) ;
#6702 = FACE_OUTER_BOUND ( 'NONE', #5537, .T. ) ;
#6703 = ORIENTED_EDGE ( 'NONE', *, *, #11235, .T. ) ;
#6704 = EDGE_CURVE ( 'NONE', #18610, #421, #13492, .T. ) ;
#6705 = CARTESIAN_POINT ( 'NONE',  ( 3.950837973638668288, 0.000000000000000000, 0.000000000000000000 ) ) ;
#6706 = FACE_OUTER_BOUND ( 'NONE', #11255, .T. ) ;
#6707 = EDGE_CURVE ( 'NONE', #13827, #16117, #2381, .T. ) ;
#6708 = ORIENTED_EDGE ( 'NONE', *, *, #18094, .T. ) ;
#6709 = DIRECTION ( 'NONE',  ( 0.000000000000000000, 0.000000000000000000, -1.000000000000000000 ) ) ;
#6710 = VECTOR ( 'NONE', #10899, 1000.000000000000000 ) ;
#6711 = CARTESIAN_POINT ( 'NONE',  ( 0.4862570985993235340, 13.89016912371017476, -0.7479633556562934604 ) ) ;
#6712 = EDGE_CURVE ( 'NONE', #12585, #6128, #12902, .T. ) ;
#6713 = CARTESIAN_POINT ( 'NONE',  ( 3.950837973638676281, 14.31366178983253512, 2.591948120961855118 ) ) ;
#6714 = CARTESIAN_POINT ( 'NONE',  ( 1.846524061778019199, 10.27028962889607477, -7.023652644192158512 ) ) ;
#6715 = DIRECTION ( 'NONE',  ( 0.000000000000000000, -1.000000000000000000, -0.000000000000000000 ) ) ;
#6716 = CIRCLE ( 'NONE', #18902, 2.375000000000000444 ) ;
#6717 = CARTESIAN_POINT ( 'NONE',  ( 1.977228804422745068, 3.321884655131805975, -15.04020501276218091 ) ) ;
#6718 = CARTESIAN_POINT ( 'NONE',  ( 16.56753206892534891, -0.001421777558676017277, 0.009389754735542238384 ) ) ;
#6720 = EDGE_LOOP ( 'NONE', ( #12578, #14239, #10892, #8230 ) ) ;
#6719 = DIRECTION ( 'NONE',  ( -1.000000000000000000, 0.000000000000000000, -0.000000000000000000 ) ) ;
#6721 = LINE ( 'NONE', #11023, #5405 ) ;
#6722 = FACE_OUTER_BOUND ( 'NONE', #7108, .T. ) ;
#6723 = CARTESIAN_POINT ( 'NONE',  ( 0.3307726912345205772, 8.558645027434268471, 10.76786801061209964 ) ) ;
#6724 = CARTESIAN_POINT ( 'NONE',  ( 0.3137051932979757485, -4.679953077377398074, -12.91601973349275134 ) ) ;
#6725 = ORIENTED_EDGE ( 'NONE', *, *, #13748, .F. ) ;
#6726 = ORIENTED_EDGE ( 'NONE', *, *, #581, .F. ) ;
#6727 = CARTESIAN_POINT ( 'NONE',  ( 0.3137051932979792457, 8.442169467527008919, -10.83767969834794087 ) ) ;
#6728 = DIRECTION ( 'NONE',  ( 0.000000000000000000, -1.000000000000000000, 0.000000000000000000 ) ) ;
#6729 = EDGE_LOOP ( 'NONE', ( #6042, #7134, #8063, #8870, #4269, #13753 ) ) ;
#6730 = CARTESIAN_POINT ( 'NONE',  ( 0.3137051932979809665, -4.679953077377580151, 12.91601973349268917 ) ) ;
#6731 = EDGE_CURVE ( 'NONE', #8559, #12766, #8304, .T. ) ;
#6732 = PRESENTATION_STYLE_ASSIGNMENT (( #6815 ) ) ;
#6733 = ADVANCED_FACE ( 'NONE', ( #5802 ), #4045, .F. ) ;
#6734 = CARTESIAN_POINT ( 'NONE',  ( 1.847461586945727152, -10.08650590720931284, -7.286856109515166047 ) ) ;
#6735 = LINE ( 'NONE', #9315, #9013 ) ;
#6736 = CARTESIAN_POINT ( 'NONE',  ( 3.950837973638668288, 14.41405733518061538, -1.958075594453841273 ) ) ;
#6737 = B_SPLINE_CURVE_WITH_KNOTS ( 'NONE', 3,
 ( #4231, #14637, #10245, #13007, #13110, #14539 ),
 .UNSPECIFIED., .F., .F.,
 ( 4, 2, 4 ),
 ( 0.000000000000000000, 0.001657017934710630505, 0.003314035869421261011 ),
 .UNSPECIFIED. ) ;
#6738 = DIRECTION ( 'NONE',  ( -0.7635533937278216055, -0.5347026451755912957, -0.3620487483322542555 ) ) ;
#6739 = SHAPE_DEFINITION_REPRESENTATION ( #17767, #13515 ) ;
#6740 = PRESENTATION_STYLE_ASSIGNMENT (( #900 ) ) ;
#6741 = CARTESIAN_POINT ( 'NONE',  ( -66.35602477868049220, -10.00000000000000888, -153.7432847437423789 ) ) ;
#6742 = DIRECTION ( 'NONE',  ( 0.7635533937278214944, -0.6204116510013502062, 0.1790966170213858510 ) ) ;
#6743 =( BOUNDED_SURFACE ( )  B_SPLINE_SURFACE ( 3, 1, ( 
 ( #16281, #6053 ),
 ( #4814, #8908 ),
 ( #11881, #7491 ),
 ( #10546, #123 ) ),
 .UNSPECIFIED., .F., .F., .T. ) 
 B_SPLINE_SURFACE_WITH_KNOTS ( ( 4, 4 ),
 ( 2, 2 ),
 ( 0.000000000000000000, 1.000000000000000000 ),
 ( 0.000000000000000000, 1.000000000000000000 ),
 .UNSPECIFIED. ) 
 GEOMETRIC_REPRESENTATION_ITEM ( )  RATIONAL_B_SPLINE_SURFACE ( (
 ( 1.000000000000000000, 1.000000000000000000),
 ( 0.7792777138730158093, 0.9689936506012928330),
 ( 0.7792777138730158093, 0.9689936506012928330),
 ( 1.000000000000000000, 1.000000000000000000) ) ) 
 REPRESENTATION_ITEM ( '' )  SURFACE ( )  );
#6744 = FACE_OUTER_BOUND ( 'NONE', #11117, .T. ) ;
#6745 = AXIS2_PLACEMENT_3D ( 'NONE', #11589, #5641, #9953 ) ;
#6746 = CARTESIAN_POINT ( 'NONE',  ( 0.3137051932979792457, -8.442169467526928983, 10.83767969834800127 ) ) ;
#6747 = ADVANCED_FACE ( 'NONE', ( #3023 ), #18431, .T. ) ;
#6748 = CARTESIAN_POINT ( 'NONE',  ( -205.0000000000000000, 4.999999999999975131, 6.000000000000005329 ) ) ;
#6749 = DIRECTION ( 'NONE',  ( -0.7635533937278214944, 0.5347026451755939602, 0.3620487483322503142 ) ) ;
#6750 = VERTEX_POINT ( 'NONE', #17377 ) ;
#6751 = ORIENTED_EDGE ( 'NONE', *, *, #6570, .T. ) ;
#6752 = ORIENTED_EDGE ( 'NONE', *, *, #16781, .F. ) ;
#6753 = VERTEX_POINT ( 'NONE', #11556 ) ;
#6754 = CARTESIAN_POINT ( 'NONE',  ( 0.3145734862173260038, 10.93207848441433683, 8.321353293018871611 ) ) ;
#6755 = CARTESIAN_POINT ( 'NONE',  ( -5.027901255400313296, -7.500000000000000888, -16.81159201184369323 ) ) ;
#6756 = CARTESIAN_POINT ( 'NONE',  ( 1.846138399168762101, 7.646096044339892650, 9.815003036200437236 ) ) ;
#6757 = CARTESIAN_POINT ( 'NONE',  ( 16.56872352241294521, -0.01033355228142500762, -0.001442253899401184716 ) ) ;
#6758 = ADVANCED_FACE ( 'NONE', ( #4484 ), #4163, .F. ) ;
#6759 = CARTESIAN_POINT ( 'NONE',  ( 1.342453679581834924, 11.38190519890867236, -9.456403821038676938 ) ) ;
#6760 = DIRECTION ( 'NONE',  ( 0.000000000000000000, -1.000000000000000000, 0.000000000000000000 ) ) ;
#6761 = CIRCLE ( 'NONE', #14682, 11.50000000000000178 ) ;
#6762 = CARTESIAN_POINT ( 'NONE',  ( 16.57210152137263393, -0.01214401161737629908, -0.008007331252333388036 ) ) ;
#6763 = CARTESIAN_POINT ( 'NONE',  ( 0.3939822652208159193, 8.678192463540325363, -10.75310269629511950 ) ) ;
#6764 = CARTESIAN_POINT ( 'NONE',  ( 1.562796894703937678, 0.000000000000000000, -1.500000000000000000 ) ) ;
#6765 = VERTEX_POINT ( 'NONE', #13074 ) ;
#6766 = VERTEX_POINT ( 'NONE', #11464 ) ;
#6767 = EDGE_CURVE ( 'NONE', #8500, #16009, #152, .T. ) ;
#6768 = ORIENTED_EDGE ( 'NONE', *, *, #12471, .F. ) ;
#6769 = ORIENTED_EDGE ( 'NONE', *, *, #14325, .F. ) ;
#6770 = CARTESIAN_POINT ( 'NONE',  ( 16.58200780006414732, 0.01115192838421469497, -0.0006320991582341122352 ) ) ;
#6771 = VECTOR ( 'NONE', #3138, 1000.000000000000000 ) ;
#6772 = CARTESIAN_POINT ( 'NONE',  ( 0.4754618798421162973, -13.45049478164062329, 3.583352865732616355 ) ) ;
#6773 = CARTESIAN_POINT ( 'NONE',  ( 2.123976203522053741, -14.31368049382974483, 6.261444813538503240 ) ) ;
#6774 = CARTESIAN_POINT ( 'NONE',  ( 0.3058872367615226295, -8.562166468153792565, 10.75034008168912791 ) ) ;
#6775 = CYLINDRICAL_SURFACE ( 'NONE', #13951, 5.000000000000000000 ) ;
#6776 = ORIENTED_EDGE ( 'NONE', *, *, #10570, .T. ) ;
#6777 = CARTESIAN_POINT ( 'NONE',  ( 1.846955891736115740, 10.21904526726846640, 7.098901504650394934 ) ) ;
#6778 = CARTESIAN_POINT ( 'NONE',  ( 0.4862570985993235340, 13.44146924561385958, -3.580942890621532371 ) ) ;
#6779 = CARTESIAN_POINT ( 'NONE',  ( 3.601232060344256247, 7.499999999999740652, -13.21583132166216679 ) ) ;
#6780 = CARTESIAN_POINT ( 'NONE',  ( 2.002547531651519996, -6.845637710436110801, -10.57595306287299763 ) ) ;
#6781 = DIRECTION ( 'NONE',  ( -0.7561779333270775005, 0.4122479608995705536, 0.5081796452863259761 ) ) ;
#6782 = CARTESIAN_POINT ( 'NONE',  ( 1.959212340397943786, -10.53510106265286517, 6.829000156128149257 ) ) ;
#6783 = CARTESIAN_POINT ( 'NONE',  ( 1.959212340397946006, -4.509090217468600947, 11.71715421693496673 ) ) ;
#6784 = ADVANCED_FACE ( 'NONE', ( #16138 ), #11360, .T. ) ;
#6785 = ORIENTED_EDGE ( 'NONE', *, *, #17934, .F. ) ;
#6787 = ORIENTED_EDGE ( 'NONE', *, *, #12311, .T. ) ;
#6786 = CARTESIAN_POINT ( 'NONE',  ( 16.57210152137263393, -0.009075239946108286035, 0.01136813053532071717 ) ) ;
#6788 = AXIS2_PLACEMENT_3D ( 'NONE', #14532, #18733, #4225 ) ;
#6789 = CARTESIAN_POINT ( 'NONE',  ( 0.3058872367615230181, -13.24582953854922529, -3.664492643742902178 ) ) ;
#6790 = EDGE_LOOP ( 'NONE', ( #15670, #17779, #17222, #16385, #13948 ) ) ;
#6791 = CARTESIAN_POINT ( 'NONE',  ( 0.000000000000000000, 0.000000000000000000, 0.000000000000000000 ) ) ;
#6792 = CARTESIAN_POINT ( 'NONE',  ( 1.562796894703937678, 0.000000000000000000, -12.15840553252917289 ) ) ;
#6793 = ORIENTED_EDGE ( 'NONE', *, *, #14292, .F. ) ;
#6794 = CARTESIAN_POINT ( 'NONE',  ( 1.847426409206450959, -2.029922383240494730E-11, 12.44303504652081038 ) ) ;
#6795 = CARTESIAN_POINT ( 'NONE',  ( 2.320520222537543198, -15.43440824796705613, 3.126729907239071959 ) ) ;
#6796 = CARTESIAN_POINT ( 'NONE',  ( 0.3939875929385618369, 7.545068896001375869, -11.57636969881026801 ) ) ;
#6797 = CARTESIAN_POINT ( 'NONE',  ( 16.58200780006414732, 0.008650561019685530303, -0.007066318000004736047 ) ) ;
#6798 = DIRECTION ( 'NONE',  ( -0.000000000000000000, -0.000000000000000000, -1.000000000000000000 ) ) ;
#6799 = ADVANCED_FACE ( 'NONE', ( #4579 ), #1486, .F. ) ;
#6800 = CARTESIAN_POINT ( 'NONE',  ( 2.123976203522053741, -15.26039569100257509, -3.347755036806064677 ) ) ;
#6801 = EDGE_CURVE ( 'NONE', #3637, #1137, #3725, .T. ) ;
#6802 = EDGE_CURVE ( 'NONE', #5678, #9382, #14100, .T. ) ;
#6803 = DIRECTION ( 'NONE',  ( 0.000000000000000000, 0.000000000000000000, -1.000000000000000000 ) ) ;
#6805 = ORIENTED_EDGE ( 'NONE', *, *, #13397, .T. ) ;
#6804 = DIRECTION ( 'NONE',  ( -1.000000000000000000, 0.000000000000000000, 0.000000000000000000 ) ) ;
#6806 = CARTESIAN_POINT ( 'NONE',  ( 16.56679352167444819, 0.006526964904752955397, 0.006618561353599231728 ) ) ;
#6807 = ORIENTED_EDGE ( 'NONE', *, *, #13273, .T. ) ;
#6808 = CARTESIAN_POINT ( 'NONE',  ( 2.002547531651519996, 7.942910686618173344, 9.778737580845726640 ) ) ;
#6809 = CARTESIAN_POINT ( 'NONE',  ( 1.959212340397945118, 4.509090217468684436, -11.71715421693493830 ) ) ;
#6810 = EDGE_LOOP ( 'NONE', ( #180, #17862, #4599, #9469 ) ) ;
#6811 = CARTESIAN_POINT ( 'NONE',  ( 3.512766787570699822, -13.55823433651950616, -6.535475144497160827 ) ) ;
#6812 = CARTESIAN_POINT ( 'NONE',  ( 0.3137051932979809665, 10.83767969834803324, 8.442169467526891680 ) ) ;
#6813 = ORIENTED_EDGE ( 'NONE', *, *, #10539, .T. ) ;
#6814 = CARTESIAN_POINT ( 'NONE',  ( 0.3148208552358936485, 4.463611911212218786, 12.99355031785207260 ) ) ;
#6815 = SURFACE_STYLE_USAGE ( .BOTH. , #18466 ) ;
#6816 = CARTESIAN_POINT ( 'NONE',  ( 16.56872352241294521, 0.001442253899401220278, -0.01033355228142500415 ) ) ;
#6817 = DIRECTION ( 'NONE',  ( 1.000000000000000000, 0.000000000000000000, 0.000000000000000000 ) ) ;
#6818 = CARTESIAN_POINT ( 'NONE',  ( 1.861706995891668104, 12.00328602385080679, 3.332865258614018611 ) ) ;
#6819 = CIRCLE ( 'NONE', #5298, 2.500000000000000888 ) ;
#6820 = CARTESIAN_POINT ( 'NONE',  ( 3.950837973638668288, 0.000000000000000000, 0.000000000000000000 ) ) ;
#6821 = SHAPE_DEFINITION_REPRESENTATION ( #6331, #5797 ) ;
#6822 = SURFACE_STYLE_FILL_AREA ( #12642 ) ;
#6823 = CARTESIAN_POINT ( 'NONE',  ( 1.959212340397946450, 7.909199412631302550, -9.750290364083546990 ) ) ;
#6824 = CARTESIAN_POINT ( 'NONE',  ( 16.56753206892534891, 0.009369540855502532517, -0.001549402974394196693 ) ) ;
#6825 = CARTESIAN_POINT ( 'NONE',  ( 1.846524061778019199, -3.506196582971023545, -11.93805390544204670 ) ) ;
#6826 = CARTESIAN_POINT ( 'NONE',  ( 1.846822687350020198, 3.566003975885688515, 11.92063725419900777 ) ) ;
#6827 = CARTESIAN_POINT ( 'NONE',  ( 0.3095370825347233956, 13.20347358821914519, 3.806662003783457315 ) ) ;
#6828 = EDGE_CURVE ( 'NONE', #2096, #16044, #17146, .T. ) ;
#6829 = CARTESIAN_POINT ( 'NONE',  ( 8.522092701127531811, -3.777034505568479528, -5.841710761610173108 ) ) ;
#6830 = EDGE_CURVE ( 'NONE', #12767, #15590, #5159, .T. ) ;
#6831 = ORIENTED_EDGE ( 'NONE', *, *, #3891, .F. ) ;
#6832 = AXIS2_PLACEMENT_3D ( 'NONE', #7490, #16085, #17512 ) ;
#6833 = ORIENTED_EDGE ( 'NONE', *, *, #722, .F. ) ;
#6834 = AXIS2_PLACEMENT_3D ( 'NONE', #1690, #11827, #4658 ) ;
#6835 = VERTEX_POINT ( 'NONE', #6488 ) ;
#6836 = VERTEX_POINT ( 'NONE', #2100 ) ;
#6837 = EDGE_CURVE ( 'NONE', #11580, #9697, #15274, .T. ) ;
#6838 = CARTESIAN_POINT ( 'NONE',  ( -194.9999999999999716, 9.999999999999973355, 5.999999999999999112 ) ) ;
#6839 = CARTESIAN_POINT ( 'NONE',  ( 1.846822687350014869, -9.891732594446525084, -7.547953575784235092 ) ) ;
#6840 = CARTESIAN_POINT ( 'NONE',  ( 3.353306896162455697, 7.069984850384810393, 12.02594772223098651 ) ) ;
#6841 = CARTESIAN_POINT ( 'NONE',  ( 1.918921323896325193, 6.832782632379378107, 10.48468902844554052 ) ) ;
#6842 = DIRECTION ( 'NONE',  ( 1.000000000000000000, 0.000000000000000000, 0.000000000000000000 ) ) ;
#6843 = CARTESIAN_POINT ( 'NONE',  ( 16.56822296793089322, 0.01011126603341077484, -0.0007467251401297481410 ) ) ;
#6844 = AXIS2_PLACEMENT_3D ( 'NONE', #12261, #9394, #6719 ) ;
#6845 = CARTESIAN_POINT ( 'NONE',  ( 0.3151928478948589074, -0.0001388664988634735829, -13.73922860964089487 ) ) ;
#6846 = EDGE_CURVE ( 'NONE', #2316, #18014, #10752, .T. ) ;
#6847 = FACE_OUTER_BOUND ( 'NONE', #9184, .T. ) ;
#6848 = LINE ( 'NONE', #6764, #7863 ) ;
#6849 = ORIENTED_EDGE ( 'NONE', *, *, #2512, .F. ) ;
#6850 = EDGE_CURVE ( 'NONE', #14405, #14673, #6110, .T. ) ;
#6851 = ADVANCED_FACE ( 'NONE', ( #11934 ), #9357, .T. ) ;
#6852 = EDGE_LOOP ( 'NONE', ( #8991, #17405, #1392, #3496 ) ) ;
#6853 = VERTEX_POINT ( 'NONE', #13661 ) ;
#6854 = VERTEX_POINT ( 'NONE', #10607 ) ;
#6855 = FACE_OUTER_BOUND ( 'NONE', #18318, .T. ) ;
#6856 = CARTESIAN_POINT ( 'NONE',  ( 0.3095370825347234511, 7.700448427571873644, 11.38092634279631277 ) ) ;
#6857 = CARTESIAN_POINT ( 'NONE',  ( 1.918918678667048683, -11.69059232068581800, 4.466049546133867842 ) ) ;
#6858 = LINE ( 'NONE', #3985, #10252 ) ;
#6859 = ORIENTED_EDGE ( 'NONE', *, *, #4336, .F. ) ;
#6860 = CARTESIAN_POINT ( 'NONE',  ( 1.847380140988739594, 10.13114603776196887, 7.224522571381366554 ) ) ;
#6861 = VECTOR ( 'NONE', #7362, 1000.000000000000000 ) ;
#6862 = EDGE_CURVE ( 'NONE', #9401, #7021, #15416, .T. ) ;
#6863 = CARTESIAN_POINT ( 'NONE',  ( 1.847247051441594179, -11.78111530882020297, -4.004229874809150047 ) ) ;
#6864 = VECTOR ( 'NONE', #15087, 1000.000000000000000 ) ;
#6865 = CARTESIAN_POINT ( 'NONE',  ( 6.108979705494776979, 3.422227477007715013, -11.99999999936562567 ) ) ;
#6866 = CARTESIAN_POINT ( 'NONE',  ( 1.562796894703937678, 6.799999999999999822, 0.000000000000000000 ) ) ;
#6867 = CARTESIAN_POINT ( 'NONE',  ( 3.074695600507264537, -13.70113613813205689, 7.366518011945889732 ) ) ;
#6868 = CARTESIAN_POINT ( 'NONE',  ( 0.3939822652208125886, 13.34132036472942318, -3.598529276937123544 ) ) ;
#6869 = CARTESIAN_POINT ( 'NONE',  ( 16.56782317627811096, 0.009228812961908652857, -0.003357783021327854014 ) ) ;
#6870 = LINE ( 'NONE', #12693, #6969 ) ;
#6871 = ORIENTED_EDGE ( 'NONE', *, *, #16460, .T. ) ;
#6872 = AXIS2_PLACEMENT_3D ( 'NONE', #9683, #5103, #16766 ) ;
#6874 = ORIENTED_EDGE ( 'NONE', *, *, #8699, .T. ) ;
#6873 = DIRECTION ( 'NONE',  ( 0.000000000000000000, 0.000000000000000000, -1.000000000000000000 ) ) ;
#6875 = CARTESIAN_POINT ( 'NONE',  ( 0.3137051932979792457, 4.679953077377485116, 12.91601973349272114 ) ) ;
#6876 = VECTOR ( 'NONE', #12112, 1000.000000000000000 ) ;
#6877 = CARTESIAN_POINT ( 'NONE',  ( 0.4754618798421162973, -13.45049478164057177, -3.583352865732810866 ) ) ;
#6878 = ORIENTED_EDGE ( 'NONE', *, *, #18749, .T. ) ;
#6879 = DIRECTION ( 'NONE',  ( -1.000000000000000000, 0.000000000000000000, 0.000000000000000000 ) ) ;
#6880 = B_SPLINE_CURVE_WITH_KNOTS ( 'NONE', 3,
 ( #17949, #13533, #450, #12209, #10683, #6283 ),
 .UNSPECIFIED., .F., .F.,
 ( 4, 2, 4 ),
 ( 4.276569467073304015E-17, 0.0002014099069817285948, 0.0004028198139634144178 ),
 .UNSPECIFIED. ) ;
#6881 = CARTESIAN_POINT ( 'NONE',  ( 1.847168016377981559, -12.44137401948661648, 0.1868244120189130053 ) ) ;
#6882 = CARTESIAN_POINT ( 'NONE',  ( 2.636624412716062960, 2.862162146982868194, -15.80357026013419564 ) ) ;
#6883 = EDGE_LOOP ( 'NONE', ( #16436, #12948, #13260, #12348, #18305 ) ) ;
#6884 = CARTESIAN_POINT ( 'NONE',  ( 20.00000000000000000, 2.499999999999997780, -16.99999999999999645 ) ) ;
#6885 = EDGE_CURVE ( 'NONE', #1936, #4361, #5251, .T. ) ;
#6886 = CARTESIAN_POINT ( 'NONE',  ( 1.254255976357440572, -14.24071337840763363, 3.563435620217590749 ) ) ;
#6887 = CIRCLE ( 'NONE', #17567, 14.54644660717763927 ) ;
#6888 = CARTESIAN_POINT ( 'NONE',  ( 1.847247051441591514, 12.44188156437794390, 0.1676840720645733362 ) ) ;
#6889 = AXIS2_PLACEMENT_3D ( 'NONE', #5508, #4087, #15740 ) ;
#6890 = CYLINDRICAL_SURFACE ( 'NONE', #2873, 5.000000000000000888 ) ;
#6891 = B_SPLINE_CURVE_WITH_KNOTS ( 'NONE', 3,
 ( #17563, #7253, #10592, #4665, #16429, #3311 ),
 .UNSPECIFIED., .F., .F.,
 ( 4, 2, 4 ),
 ( 8.131516293641283255E-19, 0.001657017934709845109, 0.003314035869419688484 ),
 .UNSPECIFIED. ) ;
#6892 = CARTESIAN_POINT ( 'NONE',  ( 1.846138399168762989, 11.95493567637850774, 3.446241763653039580 ) ) ;
#6893 = DIRECTION ( 'NONE',  ( 0.000000000000000000, 0.000000000000000000, 1.000000000000000000 ) ) ;
#6894 = DIRECTION ( 'NONE',  ( -1.000000000000000000, -0.000000000000000000, -0.000000000000000000 ) ) ;
#6895 = DIRECTION ( 'NONE',  ( 0.000000000000000000, 0.000000000000000000, 1.000000000000000000 ) ) ;
#6897 = VERTEX_POINT ( 'NONE', #13366 ) ;
#6896 = CARTESIAN_POINT ( 'NONE',  ( 16.57778382496167424, -0.01354073047775889056, 0.006312874906844006574 ) ) ;
#6898 = DIRECTION ( 'NONE',  ( -1.000000000000000000, 0.000000000000000000, -0.000000000000000000 ) ) ;
#6899 = AXIS2_PLACEMENT_3D ( 'NONE', #8366, #13036, #11608 ) ;
#6900 = CARTESIAN_POINT ( 'NONE',  ( 3.950837973638676281, -12.81214529934970336, -6.888253895133431115 ) ) ;
#6901 = DIRECTION ( 'NONE',  ( -1.000000000000000000, 0.000000000000000000, -0.000000000000000000 ) ) ;
#6902 = VECTOR ( 'NONE', #4796, 1000.000000000000000 ) ;
#6903 = ORIENTED_EDGE ( 'NONE', *, *, #10629, .T. ) ;
#6904 = CARTESIAN_POINT ( 'NONE',  ( 1.562796894703937678, 0.000000000000000000, 0.000000000000000000 ) ) ;
#6905 = CARTESIAN_POINT ( 'NONE',  ( 2.179449471770337432, -4.500000000000000000, -6.000000000000000000 ) ) ;
#6906 = ORIENTED_EDGE ( 'NONE', *, *, #16626, .F. ) ;
#6907 = DIRECTION ( 'NONE',  ( 0.000000000000000000, 0.2588190451025206285, 0.9659258262890683122 ) ) ;
#6908 = EDGE_CURVE ( 'NONE', #6039, #2050, #18053, .T. ) ;
#6909 = EDGE_CURVE ( 'NONE', #7024, #7279, #15612, .T. ) ;
#6910 = EDGE_CURVE ( 'NONE', #12290, #5702, #3936, .T. ) ;
#6911 = FACE_OUTER_BOUND ( 'NONE', #16390, .T. ) ;
#6912 = DIRECTION ( 'NONE',  ( 0.7635533937278214944, 0.2197766120036505344, -0.6071939193889570596 ) ) ;
#6913 = CARTESIAN_POINT ( 'NONE',  ( 0.3142014840576535795, -11.33546131209467767, 7.762239086932820165 ) ) ;
#6914 = CARTESIAN_POINT ( 'NONE',  ( 3.074695600507182824, 6.754521329825023734, -14.01296402267889007 ) ) ;
#6915 = UNCERTAINTY_MEASURE_WITH_UNIT (LENGTH_MEASURE( 1.000000000000000082E-05 ), #15055, 'distance_accuracy_value', 'NONE');
#6916 = ORIENTED_EDGE ( 'NONE', *, *, #12795, .T. ) ;
#6917 =( LENGTH_UNIT ( ) NAMED_UNIT ( * ) SI_UNIT ( .MILLI., .METRE. ) );
#6918 = CARTESIAN_POINT ( 'NONE',  ( 16.56753206892534891, -0.008490833999798035742, 0.004253784598196731770 ) ) ;
#6919 = DIRECTION ( 'NONE',  ( -1.000000000000000000, -0.000000000000000000, -0.000000000000000000 ) ) ;
#6920 = EDGE_CURVE ( 'NONE', #7741, #2927, #9067, .T. ) ;
#6921 = CARTESIAN_POINT ( 'NONE',  ( 2.002547531651519996, -0.6781519942170860515, -12.57989064830760206 ) ) ;
#6922 = CARTESIAN_POINT ( 'NONE',  ( 16.56753206892534891, -0.004253784598196240843, 0.008490833999798906573 ) ) ;
#6923 = DIRECTION ( 'NONE',  ( 0.000000000000000000, 0.000000000000000000, 1.000000000000000000 ) ) ;
#6924 = AXIS2_PLACEMENT_3D ( 'NONE', #12786, #14669, #11715 ) ;
#6925 = ORIENTED_EDGE ( 'NONE', *, *, #4469, .T. ) ;
#6926 = CARTESIAN_POINT ( 'NONE',  ( 0.3151928476913523069, 11.11514699826562946, -8.075884471919630769 ) ) ;
#6927 = DIRECTION ( 'NONE',  ( 1.000000000000000000, 0.000000000000000000, 0.000000000000000000 ) ) ;
#6928 = B_SPLINE_CURVE_WITH_KNOTS ( 'NONE', 3,
 ( #3836, #2393, #7084, #8246 ),
 .UNSPECIFIED., .F., .F.,
 ( 4, 4 ),
 ( 2.359479019930958314E-17, 0.003005512676784853534 ),
 .UNSPECIFIED. ) ;
#6929 = EDGE_LOOP ( 'NONE', ( #5431, #17373, #280, #13218 ) ) ;
#6930 = CONICAL_SURFACE ( 'NONE', #4807, 14.54644660717763927, 0.8559913436420816257 ) ;
#6931 = VECTOR ( 'NONE', #10960, 1000.000000000000227 ) ;
#6932 = ORIENTED_EDGE ( 'NONE', *, *, #13490, .F. ) ;
#6933 = ORIENTED_EDGE ( 'NONE', *, *, #15837, .T. ) ;
#6934 =( GEOMETRIC_REPRESENTATION_CONTEXT ( 3 ) GLOBAL_UNCERTAINTY_ASSIGNED_CONTEXT ( ( #1573 ) ) GLOBAL_UNIT_ASSIGNED_CONTEXT ( ( #18630, #18272, #15490 ) ) REPRESENTATION_CONTEXT ( 'NONE', 'WORKASPACE' ) );
#6935 = B_SPLINE_CURVE_WITH_KNOTS ( 'NONE', 3,
 ( #959, #3922, #1041, #18173, #15483, #10923 ),
 .UNSPECIFIED., .F., .F.,
 ( 4, 2, 4 ),
 ( 0.000000000000000000, 0.001656992708822831520, 0.003313985417645663040 ),
 .UNSPECIFIED. ) ;
#6936 = ORIENTED_EDGE ( 'NONE', *, *, #5449, .T. ) ;
#6937 = CIRCLE ( 'NONE', #1431, 2.100000000000000977 ) ;
#6938 = VECTOR ( 'NONE', #4704, 1000.000000000000114 ) ;
#6939 = CARTESIAN_POINT ( 'NONE',  ( 2.636624412714236865, 0.000000000000000000, 0.000000000000000000 ) ) ;
#6940 = CARTESIAN_POINT ( 'NONE',  ( 16.56782317627811096, 0.009814734722107082768, 0.0003415813796006631126 ) ) ;
#6941 = ADVANCED_FACE ( 'NONE', ( #575 ), #15022, .T. ) ;
#6942 = VECTOR ( 'NONE', #3090, 1000.000000000000000 ) ;
#6943 =( REPRESENTATION_RELATIONSHIP ('NONE','NONE', #5200, #9604 ) REPRESENTATION_RELATIONSHIP_WITH_TRANSFORMATION ( #5468 )SHAPE_REPRESENTATION_RELATIONSHIP( ) );
#6944 = DIRECTION ( 'NONE',  ( 0.000000000000000000, 0.000000000000000000, 1.000000000000000000 ) ) ;
#6945 = CARTESIAN_POINT ( 'NONE',  ( -199.9999999999999716, -5.000000000000024869, 6.000000000000000000 ) ) ;
#6946 = AXIS2_PLACEMENT_3D ( 'NONE', #13286, #17595, #5729 ) ;
#6947 = CARTESIAN_POINT ( 'NONE',  ( -194.9999999999999716, -5.000000000000024869, 6.000000000000005329 ) ) ;
#6948 = CARTESIAN_POINT ( 'NONE',  ( 0.3939875929385670550, -12.90850834464103691, 4.930599594904505167 ) ) ;
#6949 = CARTESIAN_POINT ( 'NONE',  ( 16.58200780006414732, -0.01080144354108990290, 0.002844973367390998473 ) ) ;
#6950 = CARTESIAN_POINT ( 'NONE',  ( 0.3151930723728423867, -13.09040889075573411, 4.172946285306520231 ) ) ;
#6951 = CARTESIAN_POINT ( 'NONE',  ( -199.9999999999999716, 9.999999999999973355, 6.000000000000000000 ) ) ;
#6952 = EDGE_CURVE ( 'NONE', #2439, #1448, #1597, .T. ) ;
#6953 = ORIENTED_EDGE ( 'NONE', *, *, #8829, .F. ) ;
#6954 = ORIENTED_EDGE ( 'NONE', *, *, #4018, .T. ) ;
#6955 = CIRCLE ( 'NONE', #2661, 0.5000000000000004441 ) ;
#6956 = VERTEX_POINT ( 'NONE', #13926 ) ;
#6957 = ORIENTED_EDGE ( 'NONE', *, *, #11417, .T. ) ;
#6958 = ORIENTED_EDGE ( 'NONE', *, *, #11334, .F. ) ;
#6959 = DIRECTION ( 'NONE',  ( -1.000000000000000000, 0.000000000000000000, 0.000000000000000000 ) ) ;
#6960 = CARTESIAN_POINT ( 'NONE',  ( 2.002547531651519996, -11.75462648437098601, -4.532360870844453160 ) ) ;
#6961 = CARTESIAN_POINT ( 'NONE',  ( 1.846955891736115518, 9.909315188408152508, -7.525208385419853485 ) ) ;
#6962 = LINE ( 'NONE', #11079, #5366 ) ;
#6963 = CARTESIAN_POINT ( 'NONE',  ( 0.000000000000000000, 0.000000000000000000, 0.000000000000000000 ) ) ;
#6964 = VERTEX_POINT ( 'NONE', #8118 ) ;
#6965 = CARTESIAN_POINT ( 'NONE',  ( 16.56872352241294521, 0.001821578298044641397, 0.01027347319884442528 ) ) ;
#6966 = DIRECTION ( 'NONE',  ( 0.7635533937278214944, 0.6204116510013490959, -0.1790966170213899034 ) ) ;
#6967 = CARTESIAN_POINT ( 'NONE',  ( 1.329448181772381776, 7.500000000000063949, -13.08538760542143464 ) ) ;
#6968 = DIRECTION ( 'NONE',  ( 1.000000000000000000, 0.000000000000000000, 0.000000000000000000 ) ) ;
#6969 = VECTOR ( 'NONE', #18524, 1000.000000000000000 ) ;
#6970 = CARTESIAN_POINT ( 'NONE',  ( 0.3939875929385628361, -8.678227324501040840, -10.75308190953752785 ) ) ;
#6971 = CARTESIAN_POINT ( 'NONE',  ( 0.4385251269669947494, 13.39302348765813910, -3.577373010348575910 ) ) ;
#6972 = CARTESIAN_POINT ( 'NONE',  ( 1.560000000000000053, 0.8660254037844389297, -1.500000000000000000 ) ) ;
#6973 = EDGE_CURVE ( 'NONE', #3136, #1746, #8919, .T. ) ;
#6974 = DIRECTION ( 'NONE',  ( 0.000000000000000000, 0.000000000000000000, -1.000000000000000000 ) ) ;
#6975 = ORIENTED_EDGE ( 'NONE', *, *, #10269, .F. ) ;
#6976 = AXIS2_PLACEMENT_3D ( 'NONE', #7792, #6061, #17819 ) ;
#6978 = ORIENTED_EDGE ( 'NONE', *, *, #17310, .F. ) ;
#6977 = FACE_OUTER_BOUND ( 'NONE', #9251, .T. ) ;
#6979 = LINE ( 'NONE', #15292, #8149 ) ;
#6980 = EDGE_CURVE ( 'NONE', #15773, #678, #13185, .T. ) ;
#6981 = CARTESIAN_POINT ( 'NONE',  ( 16.56872352241294521, 0.004564908236400220913, 0.009382111268606271176 ) ) ;
#6982 = ORIENTED_EDGE ( 'NONE', *, *, #12536, .T. ) ;
#6983 = LINE ( 'NONE', #8785, #10051 ) ;
#6984 = CARTESIAN_POINT ( 'NONE',  ( -6.538348415310987427, -2.500000000000060396, -12.00000000000000000 ) ) ;
#6985 = CARTESIAN_POINT ( 'NONE',  ( 0.4754618798421167414, 13.45049478164064638, -3.583352865732531534 ) ) ;
#6986 = SURFACE_SIDE_STYLE ('',( #1142 ) ) ;
#6987 = ORIENTED_EDGE ( 'NONE', *, *, #1975, .T. ) ;
#6988 = FACE_OUTER_BOUND ( 'NONE', #13385, .T. ) ;
#6989 = DIRECTION ( 'NONE',  ( 0.000000000000000000, 0.000000000000000000, 1.000000000000000000 ) ) ;
#6990 = CARTESIAN_POINT ( 'NONE',  ( 0.3308579732647025651, -13.74211098745268522, -0.5950689966505779971 ) ) ;
#6991 = PLANE ( 'NONE',  #8694 ) ;
#6992 = DIRECTION ( 'NONE',  ( -0.000000000000000000, -0.000000000000000000, 1.000000000000000000 ) ) ;
#6993 = EDGE_CURVE ( 'NONE', #12620, #11032, #12403, .T. ) ;
#6994 = DIRECTION ( 'NONE',  ( 0.000000000000000000, 8.673617379884033500E-16, -1.000000000000000000 ) ) ;
#6995 = CARTESIAN_POINT ( 'NONE',  ( -2.749999999999996891, 3.367778697655217067E-16, -6.000000000000000888 ) ) ;
#6997 = VERTEX_POINT ( 'NONE', #6677 ) ;
#6996 = PLANE ( 'NONE',  #12425 ) ;
#6998 = EDGE_CURVE ( 'NONE', #6128, #3394, #17155, .T. ) ;
#6999 = CARTESIAN_POINT ( 'NONE',  ( 2.705023505549866591, -11.23800170568051371, -7.115606223895292182 ) ) ;
#7000 = ORIENTED_EDGE ( 'NONE', *, *, #9289, .T. ) ;
#7001 = CARTESIAN_POINT ( 'NONE',  ( 3.074695600507147297, -15.41438262616236088, -2.093687500612132268 ) ) ;
#7002 = DIRECTION ( 'NONE',  ( 1.000000000000000000, 0.000000000000000000, 0.000000000000000000 ) ) ;
#7003 = VERTEX_POINT ( 'NONE', #2607 ) ;
#7004 = CARTESIAN_POINT ( 'NONE',  ( 0.3142011359265368120, 4.608101617236774139, 12.94258167753013922 ) ) ;
#7005 = CYLINDRICAL_SURFACE ( 'NONE', #11892, 4.999999999999997335 ) ;
#7006 = DIRECTION ( 'NONE',  ( 0.7635533937278216055, 0.1790966170213880715, 0.6204116510013496510 ) ) ;
#7007 = CARTESIAN_POINT ( 'NONE',  ( 0.3148213771069364175, -11.24846294176317407, 7.888490156175182122 ) ) ;
#7009 = LINE ( 'NONE', #3853, #11501 ) ;
#7008 = AXIS2_PLACEMENT_3D ( 'NONE', #8617, #2860, #11588 ) ;
#7010 = B_SPLINE_CURVE_WITH_KNOTS ( 'NONE', 3,
 ( #8770, #5506, #1504, #18887 ),
 .UNSPECIFIED., .F., .F.,
 ( 4, 4 ),
 ( 3.019714627835872489E-16, 0.002004993803842318283 ),
 .UNSPECIFIED. ) ;
#7011 = ORIENTED_EDGE ( 'NONE', *, *, #12790, .T. ) ;
#7012 = ITEM_DEFINED_TRANSFORMATION ( 'NONE', 'NONE', #10597,  #2030 ) ;
#7013 =( BOUNDED_SURFACE ( )  B_SPLINE_SURFACE ( 3, 1, ( 
 ( #3437, #9272 ),
 ( #15104, #7438 ),
 ( #2913, #5789 ),
 ( #3204, #1506 ) ),
 .UNSPECIFIED., .F., .F., .T. ) 
 B_SPLINE_SURFACE_WITH_KNOTS ( ( 4, 4 ),
 ( 2, 2 ),
 ( 0.000000000000000000, 1.000000000000000000 ),
 ( 0.000000000000000000, 1.000000000000000000 ),
 .UNSPECIFIED. ) 
 GEOMETRIC_REPRESENTATION_ITEM ( )  RATIONAL_B_SPLINE_SURFACE ( (
 ( 1.000000000000000000, 1.000000000000000000),
 ( 0.7792777138730160313, 0.9689936506012927220),
 ( 0.7792777138730160313, 0.9689936506012927220),
 ( 1.000000000000000000, 1.000000000000000000) ) ) 
 REPRESENTATION_ITEM ( '' )  SURFACE ( )  );
#7014 = VECTOR ( 'NONE', #13132, 1000.000000000000000 ) ;
#7015 = DIRECTION ( 'NONE',  ( 0.000000000000000000, 0.000000000000000000, 1.000000000000000000 ) ) ;
#7016 = CARTESIAN_POINT ( 'NONE',  ( 0.000000000000000000, 0.000000000000000000, -6.000000000000000888 ) ) ;
#7017 = DIRECTION ( 'NONE',  ( -0.000000000000000000, -1.000000000000000000, -0.000000000000000000 ) ) ;
#7018 = CARTESIAN_POINT ( 'NONE',  ( 3.950837973638676281, -14.41405733518059229, -1.958075594453940971 ) ) ;
#7019 = CARTESIAN_POINT ( 'NONE',  ( 2.426025403784448642, 2.168404344971008868E-16, 0.000000000000000000 ) ) ;
#7020 = EDGE_CURVE ( 'NONE', #17016, #6836, #12881, .T. ) ;
#7021 = VERTEX_POINT ( 'NONE', #842 ) ;
#7022 = CARTESIAN_POINT ( 'NONE',  ( -110.6103749397691729, -82.42962774651277869, -84.79685296320238308 ) ) ;
#7023 = DIRECTION ( 'NONE',  ( 0.7071067818211358436, 0.000000000000000000, -0.7071067805519591909 ) ) ;
#7024 = VERTEX_POINT ( 'NONE', #17433 ) ;
#7025 = ORIENTED_EDGE ( 'NONE', *, *, #13628, .F. ) ;
#7026 = ORIENTED_EDGE ( 'NONE', *, *, #13916, .F. ) ;
#7027 = CARTESIAN_POINT ( 'NONE',  ( 0.3095370825347234511, -13.73357284481724427, -0.4597470195091644674 ) ) ;
#7028 = EDGE_LOOP ( 'NONE', ( #5166, #743, #18234, #16314 ) ) ;
#7029 = LINE ( 'NONE', #2514, #17907 ) ;
#7030 = CARTESIAN_POINT ( 'NONE',  ( 3.686287386450715076E-15, -27.00000000000000000, 25.01316734529526187 ) ) ;
#7031 = LINE ( 'NONE', #9786, #1062 ) ;
#7032 = CARTESIAN_POINT ( 'NONE',  ( 8.522092701127531811, 6.946128462138595694, -0.3779863304871462493 ) ) ;
#7033 = DIRECTION ( 'NONE',  ( 2.775557561562891351E-15, 0.000000000000000000, -1.000000000000000000 ) ) ;
#7034 = CARTESIAN_POINT ( 'NONE',  ( 16.56679352167444819, -0.009170718284672554205, 0.001518074900131824228 ) ) ;
#7035 = CARTESIAN_POINT ( 'NONE',  ( 0.3151926232592480726, -0.07678256780548071980, -13.73922722301401578 ) ) ;
#7036 = CARTESIAN_POINT ( 'NONE',  ( 0.4754618798421162973, -12.98792082933648118, 5.007009103465200894 ) ) ;
#7037 = ADVANCED_FACE ( 'NONE', ( #14464 ), #6632, .F. ) ;
#7038 = CARTESIAN_POINT ( 'NONE',  ( 8.438534575730034959, 2.341351102130369011, -6.454982381540262715 ) ) ;
#7039 = EDGE_CURVE ( 'NONE', #10260, #10485, #2215, .T. ) ;
#7040 = EDGE_LOOP ( 'NONE', ( #4316, #945, #13433, #18455 ) ) ;
#7041 = EDGE_CURVE ( 'NONE', #415, #1445, #6000, .T. ) ;
#7042 = ORIENTED_EDGE ( 'NONE', *, *, #18832, .T. ) ;
#7043 = ORIENTED_EDGE ( 'NONE', *, *, #5286, .T. ) ;
#7044 = ORIENTED_EDGE ( 'NONE', *, *, #11516, .T. ) ;
#7045 =( BOUNDED_SURFACE ( )  B_SPLINE_SURFACE ( 3, 1, ( 
 ( #9609, #11335 ),
 ( #8552, #1193 ),
 ( #14376, #7124 ),
 ( #15438, #3968 ) ),
 .UNSPECIFIED., .F., .F., .T. ) 
 B_SPLINE_SURFACE_WITH_KNOTS ( ( 4, 4 ),
 ( 2, 2 ),
 ( 0.000000000000000000, 1.000000000000000000 ),
 ( 0.000000000000000000, 1.000000000000000000 ),
 .UNSPECIFIED. ) 
 GEOMETRIC_REPRESENTATION_ITEM ( )  RATIONAL_B_SPLINE_SURFACE ( (
 ( 1.000000000000000000, 1.000000000000000000),
 ( 0.9933953342250436691, 0.8357391271907733676),
 ( 0.9933953342250436691, 0.8357391271907733676),
 ( 1.000000000000000000, 1.000000000000000000) ) ) 
 REPRESENTATION_ITEM ( '' )  SURFACE ( )  );
#7046 = ORIENTED_EDGE ( 'NONE', *, *, #14186, .F. ) ;
#7047 =( BOUNDED_SURFACE ( )  B_SPLINE_SURFACE ( 3, 1, ( 
 ( #9147, #3400 ),
 ( #13640, #5882 ),
 ( #2344, #7921 ),
 ( #15167, #8097 ) ),
 .UNSPECIFIED., .F., .F., .T. ) 
 B_SPLINE_SURFACE_WITH_KNOTS ( ( 4, 4 ),
 ( 2, 2 ),
 ( 0.000000000000000000, 1.000000000000000000 ),
 ( 0.000000000000000000, 1.000000000000000000 ),
 .UNSPECIFIED. ) 
 GEOMETRIC_REPRESENTATION_ITEM ( )  RATIONAL_B_SPLINE_SURFACE ( (
 ( 1.000000000000000000, 1.000000000000000000),
 ( 0.9933953342250436691, 0.8357391271907733676),
 ( 0.9933953342250436691, 0.8357391271907733676),
 ( 1.000000000000000000, 1.000000000000000000) ) ) 
 REPRESENTATION_ITEM ( '' )  SURFACE ( )  );
#7048 = CARTESIAN_POINT ( 'NONE',  ( 1.847372867223028070, 3.945260592619209028, -11.80112642014550239 ) ) ;
#7049 = APPLICATION_CONTEXT ( 'automotive_design' ) ;
#7050 = CARTESIAN_POINT ( 'NONE',  ( 16.56782317627811096, -0.009228812961909619098, -0.003357783021327203059 ) ) ;
#7051 = CARTESIAN_POINT ( 'NONE',  ( 8.522092701127531811, 0.3779863304872196350, -6.946128462138591253 ) ) ;
#7052 = ORIENTED_EDGE ( 'NONE', *, *, #3302, .F. ) ;
#7053 = CARTESIAN_POINT ( 'NONE',  ( 0.8740779401507798863, 5.211551231203803702, 13.31469722824348878 ) ) ;
#7054 = CARTESIAN_POINT ( 'NONE',  ( -194.9999999999999716, 9.999999999999976907, 6.000000000000005329 ) ) ;
#7055 = VECTOR ( 'NONE', #16229, 1000.000000000000000 ) ;
#7056 = CARTESIAN_POINT ( 'NONE',  ( 1.334466156054132657, 7.499999999999999112, -14.76217096505626181 ) ) ;
#7057 = CARTESIAN_POINT ( 'NONE',  ( 0.3151928476913618549, -11.11514699826556196, 8.075884471919712482 ) ) ;
#7058 = LINE ( 'NONE', #14223, #2846 ) ;
#7059 = CARTESIAN_POINT ( 'NONE',  ( 0.3132635586635980629, 4.743936529203241825, 12.89236642382223508 ) ) ;
#7060 = CARTESIAN_POINT ( 'NONE',  ( 3.950837973638668288, 0.000000000000000000, 0.000000000000000000 ) ) ;
#7061 = VERTEX_POINT ( 'NONE', #13032 ) ;
#7062 = ORIENTED_EDGE ( 'NONE', *, *, #13575, .F. ) ;
#7063 = CARTESIAN_POINT ( 'NONE',  ( 2.636624412715137922, -15.91454522070252153, 2.161493821597598508 ) ) ;
#7064 = ORIENTED_EDGE ( 'NONE', *, *, #17094, .T. ) ;
#7065 = VECTOR ( 'NONE', #18635, 1000.000000000000000 ) ;
#7066 = EDGE_CURVE ( 'NONE', #16598, #3596, #5230, .T. ) ;
#7067 = ORIENTED_EDGE ( 'NONE', *, *, #2000, .F. ) ;
#7068 = CARTESIAN_POINT ( 'NONE',  ( 1.847421816787902404, -0.02876707915213067360, 12.44300551404155541 ) ) ;
#7069 = ORIENTED_EDGE ( 'NONE', *, *, #8589, .T. ) ;
#7070 = CARTESIAN_POINT ( 'NONE',  ( -1.389456752619696367, -44.31487138727242581, 3.000000000000000000 ) ) ;
#7071 = DIRECTION ( 'NONE',  ( 1.000000000000000000, 0.000000000000000000, 0.000000000000000000 ) ) ;
#7072 = DIRECTION ( 'NONE',  ( 0.7635533937278216055, -0.5347026451755990673, 0.3620487483322425981 ) ) ;
#7073 = CARTESIAN_POINT ( 'NONE',  ( 1.847426409206471831, -0.06227732482761883653, -12.44303504652092229 ) ) ;
#7074 = ORIENTED_EDGE ( 'NONE', *, *, #18112, .T. ) ;
#7075 = CARTESIAN_POINT ( 'NONE',  ( 16.56872352241294521, -0.001821578298044716857, -0.01027347319884440967 ) ) ;
#7076 = CARTESIAN_POINT ( 'NONE',  ( 2.697797270744671128, 10.19107313879056953, 8.537712152180894520 ) ) ;
#7077 = CARTESIAN_POINT ( 'NONE',  ( 0.000000000000000000, 0.000000000000000000, -12.00000000000000000 ) ) ;
#7078 = CARTESIAN_POINT ( 'NONE',  ( 2.636624412714237309, 7.605649742761960042, 14.14563173255213613 ) ) ;
#7079 = CARTESIAN_POINT ( 'NONE',  ( 0.3137051932979792457, -8.442169467526928983, 10.83767969834800127 ) ) ;
#7080 = SURFACE_SIDE_STYLE ('',( #8332 ) ) ;
#7081 = DIRECTION ( 'NONE',  ( 1.000000000000000000, 0.000000000000000000, 0.000000000000000000 ) ) ;
#7082 = AXIS2_PLACEMENT_3D ( 'NONE', #5252, #11095, #16913 ) ;
#7083 = EDGE_CURVE ( 'NONE', #1012, #447, #4155, .T. ) ;
#7084 = CARTESIAN_POINT ( 'NONE',  ( 2.705023505549863039, 10.24007717649592841, -8.489131503859667305 ) ) ;
#7086 = ORIENTED_EDGE ( 'NONE', *, *, #15625, .T. ) ;
#7085 = DIRECTION ( 'NONE',  ( 0.000000000000000000, 0.000000000000000000, -1.000000000000000000 ) ) ;
#7087 = CARTESIAN_POINT ( 'NONE',  ( 0.3148213771069372502, 8.260246460850879657, -10.97836617636215628 ) ) ;
#7088 = ORIENTED_EDGE ( 'NONE', *, *, #8814, .T. ) ;
#7089 = EDGE_CURVE ( 'NONE', #11470, #8138, #18322, .T. ) ;
#7090 = FACE_OUTER_BOUND ( 'NONE', #3165, .T. ) ;
#7091 = ORIENTED_EDGE ( 'NONE', *, *, #18860, .F. ) ;
#7092 = CARTESIAN_POINT ( 'NONE',  ( 1.847247051441594179, 9.967131402978196775, 7.448813758297206711 ) ) ;
#7093 = CARTESIAN_POINT ( 'NONE',  ( 2.123976203522053741, 15.54801196254787143, -1.531817366691807125 ) ) ;
#7094 = ORIENTED_EDGE ( 'NONE', *, *, #246, .F. ) ;
#7095 = SURFACE_SIDE_STYLE ('',( #16069 ) ) ;
#7096 = CARTESIAN_POINT ( 'NONE',  ( 0.4384471787762814210, -3.577367180593642892, 13.39294437382617353 ) ) ;
#7097 = AXIS2_PLACEMENT_3D ( 'NONE', #4768, #14987, #10794 ) ;
#7098 = CARTESIAN_POINT ( 'NONE',  ( 1.977436885025100510, 3.321781585409006698, 15.04044112860174209 ) ) ;
#7099 = CARTESIAN_POINT ( 'NONE',  ( 0.3095370825347234511, -13.73357284481724427, -0.4597470195091644674 ) ) ;
#7100 = EDGE_CURVE ( 'NONE', #5854, #18437, #9537, .T. ) ;
#7101 = EDGE_LOOP ( 'NONE', ( #7074, #521 ) ) ;
#7102 = COLOUR_RGB ( '', 0.09019608, 0.27058824, 0.51372549) ;
#7103 = DIRECTION ( 'NONE',  ( 0.000000000000000000, 0.000000000000000000, 1.000000000000000000 ) ) ;
#7104 = CARTESIAN_POINT ( 'NONE',  ( 3.664313757352971823, -13.97913389346635427, 2.831308606787193316 ) ) ;
#7105 = DIRECTION ( 'NONE',  ( -1.000000000000000000, -0.000000000000000000, -0.000000000000000000 ) ) ;
#7106 = CARTESIAN_POINT ( 'NONE',  ( 1.342453679581834924, 11.38190519890853558, 9.456403821038842139 ) ) ;
#7107 = CARTESIAN_POINT ( 'NONE',  ( 6.000000000000000888, 17.00000000000000000, 4.000000000000000000 ) ) ;
#7108 = EDGE_LOOP ( 'NONE', ( #14104, #10012, #15317, #15968 ) ) ;
#7109 = CARTESIAN_POINT ( 'NONE',  ( 0.8740779401509238822, -13.83508928787439096, -3.609949156401517367 ) ) ;
#7110 = DIRECTION ( 'NONE',  ( 0.000000000000000000, 0.000000000000000000, -1.000000000000000000 ) ) ;
#7111 = ORIENTED_EDGE ( 'NONE', *, *, #1806, .T. ) ;
#7112 = ORIENTED_EDGE ( 'NONE', *, *, #8906, .F. ) ;
#7113 = CARTESIAN_POINT ( 'NONE',  ( 16.57778382496167424, -0.001819584982831791388, -0.01482878558584694619 ) ) ;
#7114 = ORIENTED_EDGE ( 'NONE', *, *, #2377, .T. ) ;
#7115 = CARTESIAN_POINT ( 'NONE',  ( 16.56822296793089322, 0.007741272030791174728, -0.006547366384936662183 ) ) ;
#7116 = ORIENTED_EDGE ( 'NONE', *, *, #8349, .T. ) ;
#7117 = EDGE_CURVE ( 'NONE', #13343, #5119, #16935, .T. ) ;
#7118 = AXIS2_PLACEMENT_3D ( 'NONE', #1643, #10250, #2966 ) ;
#7119 = B_SPLINE_CURVE_WITH_KNOTS ( 'NONE', 3,
 ( #6400, #17970, #18242, #16620 ),
 .UNSPECIFIED., .F., .F.,
 ( 4, 4 ),
 ( 0.000000000000000000, 0.002004993803840905784 ),
 .UNSPECIFIED. ) ;
#7120 = CARTESIAN_POINT ( 'NONE',  ( 16.57605080000000086, 0.000000000000000000, 0.000000000000000000 ) ) ;
#7121 =( BOUNDED_SURFACE ( )  B_SPLINE_SURFACE ( 3, 1, ( 
 ( #13117, #11682 ),
 ( #3162, #13306 ),
 ( #6052, #14836 ),
 ( #4526, #10155 ) ),
 .UNSPECIFIED., .F., .F., .T. ) 
 B_SPLINE_SURFACE_WITH_KNOTS ( ( 4, 4 ),
 ( 2, 2 ),
 ( 0.000000000000000000, 1.000000000000000000 ),
 ( 0.000000000000000000, 1.000000000000000000 ),
 .UNSPECIFIED. ) 
 GEOMETRIC_REPRESENTATION_ITEM ( )  RATIONAL_B_SPLINE_SURFACE ( (
 ( 1.000000000000000000, 1.000000000000000000),
 ( 0.7792777138730158093, 0.9689936506012928330),
 ( 0.7792777138730158093, 0.9689936506012928330),
 ( 1.000000000000000000, 1.000000000000000000) ) ) 
 REPRESENTATION_ITEM ( '' )  SURFACE ( )  );
#7122 = CARTESIAN_POINT ( 'NONE',  ( 0.3150686449036065317, 13.01866258978842694, -4.391272911157185099 ) ) ;
#7123 = ADVANCED_FACE ( 'NONE', ( #5140 ), #13927, .F. ) ;
#7124 = CARTESIAN_POINT ( 'NONE',  ( 0.3720661004400037664, 4.951033743989821545, -12.89739157014187221 ) ) ;
#7125 = CARTESIAN_POINT ( 'NONE',  ( 0.3058872367615230181, -7.578326039752686150, 11.46514199369355325 ) ) ;
#7126 = FACE_OUTER_BOUND ( 'NONE', #18557, .T. ) ;
#7127 = CARTESIAN_POINT ( 'NONE',  ( 0.3939875929385618369, 7.545068896001375869, -11.57636969881026801 ) ) ;
#7128 = DIRECTION ( 'NONE',  ( 0.000000000000000000, 0.000000000000000000, 1.000000000000000000 ) ) ;
#7129 = CARTESIAN_POINT ( 'NONE',  ( 16.58200780006414732, 0.009393638146079845430, -0.006043560077721606832 ) ) ;
#7130 = CARTESIAN_POINT ( 'NONE',  ( 16.56822296793089322, -0.009385634690642031749, 0.003834730849371980905 ) ) ;
#7131 = CIRCLE ( 'NONE', #12602, 5.000000000000000888 ) ;
#7132 = AXIS2_PLACEMENT_3D ( 'NONE', #1787, #1683, #13345 ) ;
#7133 = VERTEX_POINT ( 'NONE', #235 ) ;
#7134 = ORIENTED_EDGE ( 'NONE', *, *, #18587, .T. ) ;
#7135 = ORIENTED_EDGE ( 'NONE', *, *, #984, .F. ) ;
#7136 = VERTEX_POINT ( 'NONE', #10359 ) ;
#7137 = EDGE_LOOP ( 'NONE', ( #17451, #18344, #6111, #5183 ) ) ;
#7138 = CARTESIAN_POINT ( 'NONE',  ( 1.846138399168762101, 4.238866729160568170, -11.69739621335917690 ) ) ;
#7139 = CARTESIAN_POINT ( 'NONE',  ( 1.254009781011992342, -5.487405433548717681, -13.61532727684465982 ) ) ;
#7140 = FACE_OUTER_BOUND ( 'NONE', #13932, .T. ) ;
#7141 = ORIENTED_EDGE ( 'NONE', *, *, #2353, .F. ) ;
#7142 = CARTESIAN_POINT ( 'NONE',  ( 3.377929128793398128, -13.64476897106782083, -3.070552481925011179 ) ) ;
#7143 = ADVANCED_FACE ( 'NONE', ( #16189 ), #13414, .F. ) ;
#7144 = EDGE_CURVE ( 'NONE', #12951, #5087, #10766, .T. ) ;
#7145 = CARTESIAN_POINT ( 'NONE',  ( 0.3137051932979792457, 13.73004976592202198, 0.4596302728640249136 ) ) ;
#7146 = EDGE_CURVE ( 'NONE', #10284, #7547, #11929, .T. ) ;
#7147 = CIRCLE ( 'NONE', #9868, 2.375000000000000444 ) ;
#7148 = CIRCLE ( 'NONE', #740, 13.42403576283810906 ) ;
#7149 = CARTESIAN_POINT ( 'NONE',  ( 0.7597029211760544243, 7.499999999999999112, -14.39758526244293790 ) ) ;
#7150 = CARTESIAN_POINT ( 'NONE',  ( 2.002547531651519996, -10.57595306287296921, 6.845637710436153434 ) ) ;
#7151 = CARTESIAN_POINT ( 'NONE',  ( 1.342453679581834924, -14.76648944001040142, 0.9602753779830212055 ) ) ;
#7152 = CARTESIAN_POINT ( 'NONE',  ( 0.3308579732647022875, 13.25341063505880967, -3.680601586799737923 ) ) ;
#7153 = DIRECTION ( 'NONE',  ( 1.000000000000000000, 0.000000000000000000, -0.000000000000000000 ) ) ;
#7154 = DIRECTION ( 'NONE',  ( 1.000000000000000000, 0.000000000000000000, 0.000000000000000000 ) ) ;
#7155 = EDGE_LOOP ( 'NONE', ( #2144, #6580, #9094, #12337 ) ) ;
#7156 = B_SPLINE_CURVE_WITH_KNOTS ( 'NONE', 3,
 ( #16463, #14721, #11866, #8992 ),
 .UNSPECIFIED., .F., .F.,
 ( 4, 4 ),
 ( 1.974081779422029518E-17, 0.003005512676784849631 ),
 .UNSPECIFIED. ) ;
#7157 =( BOUNDED_SURFACE ( )  B_SPLINE_SURFACE ( 3, 1, ( 
 ( #3657, #9488 ),
 ( #8157, #16842 ),
 ( #15310, #3560 ),
 ( #614, #4098 ) ),
 .UNSPECIFIED., .F., .F., .T. ) 
 B_SPLINE_SURFACE_WITH_KNOTS ( ( 4, 4 ),
 ( 2, 2 ),
 ( 0.000000000000000000, 1.000000000000000000 ),
 ( 0.000000000000000000, 1.000000000000000000 ),
 .UNSPECIFIED. ) 
 GEOMETRIC_REPRESENTATION_ITEM ( )  RATIONAL_B_SPLINE_SURFACE ( (
 ( 1.000000000000000000, 1.000000000000000000),
 ( 0.9593108457356467333, 0.9995965569486454649),
 ( 0.9593108457356467333, 0.9995965569486454649),
 ( 1.000000000000000000, 1.000000000000000000) ) ) 
 REPRESENTATION_ITEM ( '' )  SURFACE ( )  );
#7158 = EDGE_CURVE ( 'NONE', #6426, #1712, #11988, .T. ) ;
#7159 = EDGE_LOOP ( 'NONE', ( #15750, #6055, #113, #3748 ) ) ;
#7160 = CARTESIAN_POINT ( 'NONE',  ( 0.000000000000000000, 0.8660254037844389297, 1.500000000000000000 ) ) ;
#7161 = ORIENTED_EDGE ( 'NONE', *, *, #18031, .T. ) ;
#7162 = EDGE_LOOP ( 'NONE', ( #5443, #9206, #1655, #4254 ) ) ;
#7163 = DIRECTION ( 'NONE',  ( -0.000000000000000000, 1.000000000000000000, -0.000000000000000000 ) ) ;
#7164 = EDGE_LOOP ( 'NONE', ( #14395, #8002, #10059 ) ) ;
#7165 = DIRECTION ( 'NONE',  ( -1.000000000000000000, 0.000000000000000000, 0.000000000000000000 ) ) ;
#7166 = AXIS2_PLACEMENT_3D ( 'NONE', #576, #5142, #15453 ) ;
#7167 = DIRECTION ( 'NONE',  ( 0.000000000000000000, -0.000000000000000000, -1.000000000000000000 ) ) ;
#7168 = CARTESIAN_POINT ( 'NONE',  ( 20.00000000000000000, 2.499999999999998668, -12.00000000000000000 ) ) ;
#7169 = CARTESIAN_POINT ( 'NONE',  ( 0.3095370825347224519, -4.681152801286072140, -12.91933430393612703 ) ) ;
#7170 = ORIENTED_EDGE ( 'NONE', *, *, #13616, .F. ) ;
#7171 = CARTESIAN_POINT ( 'NONE',  ( 2.747332970342022840, -11.45495994260726214, 11.66639548242803492 ) ) ;
#7172 = CARTESIAN_POINT ( 'NONE',  ( 1.861706995891666105, -10.38589138506421072, -6.878962591851865760 ) ) ;
#7173 = CARTESIAN_POINT ( 'NONE',  ( 0.3150692679895994996, -13.73846569174796883, -0.1531143455845980217 ) ) ;
#7174 = DIRECTION ( 'NONE',  ( 1.540743955509788340E-33, 1.000000000000000000, 2.533398541561209262E-17 ) ) ;
#7175 = AXIS2_PLACEMENT_3D ( 'NONE', #11825, #10586, #3104 ) ;
#7176 = CARTESIAN_POINT ( 'NONE',  ( 0.4384471787762814210, -3.577367180593642892, 13.39294437382617353 ) ) ;
#7177 = CARTESIAN_POINT ( 'NONE',  ( 2.369999999999999662, 0.000000000000000000, 0.000000000000000000 ) ) ;
#7178 = ADVANCED_FACE ( 'NONE', ( #4537 ), #144, .F. ) ;
#7179 = AXIS2_PLACEMENT_3D ( 'NONE', #783, #6616, #18086 ) ;
#7180 = CONICAL_SURFACE ( 'NONE', #2586, 14.54644660717763927, 0.8559913436420816257 ) ;
#7181 = CARTESIAN_POINT ( 'NONE',  ( 0.000000000000000000, 0.000000000000000000, 0.000000000000000000 ) ) ;
#7182 = CARTESIAN_POINT ( 'NONE',  ( 2.750000000000000000, 3.306546357697853240E-16, -2.699999999999999734 ) ) ;
#7183 = ORIENTED_EDGE ( 'NONE', *, *, #9709, .T. ) ;
#7184 = CARTESIAN_POINT ( 'NONE',  ( 19.99999999999999645, 15.00000000000000000, 3.000000000000000000 ) ) ;
#7186 = ORIENTED_EDGE ( 'NONE', *, *, #7912, .F. ) ;
#7185 = DIRECTION ( 'NONE',  ( 0.000000000000000000, 0.000000000000000000, -1.000000000000000000 ) ) ;
#7187 = CARTESIAN_POINT ( 'NONE',  ( 8.438534575730034959, 5.688336279099046600, 3.845978796786057696 ) ) ;
#7188 = EDGE_CURVE ( 'NONE', #14993, #11535, #14187, .T. ) ;
#7189 = CARTESIAN_POINT ( 'NONE',  ( 0.4862570985993235340, -12.97920246947883172, 5.003653737315437944 ) ) ;
#7190 = VERTEX_POINT ( 'NONE', #17729 ) ;
#7191 = CARTESIAN_POINT ( 'NONE',  ( 2.002547531651519996, 0.6781519942171739812, 12.57989064830759851 ) ) ;
#7192 = VECTOR ( 'NONE', #213, 1000.000000000000114 ) ;
#7193 = CIRCLE ( 'NONE', #1384, 11.50000000000000178 ) ;
#7194 = VERTEX_POINT ( 'NONE', #3073 ) ;
#7195 = DIRECTION ( 'NONE',  ( -0.000000000000000000, -0.000000000000000000, 1.000000000000000000 ) ) ;
#7196 = CARTESIAN_POINT ( 'NONE',  ( 3.074695600507258320, -7.366518011946037170, 13.70113613813197873 ) ) ;
#7197 = CARTESIAN_POINT ( 'NONE',  ( 8.438534575730034959, -1.899950616255142277, -6.598402093327899287 ) ) ;
#7198 = DIRECTION ( 'NONE',  ( 0.000000000000000000, 0.000000000000000000, -1.000000000000000000 ) ) ;
#7199 = CARTESIAN_POINT ( 'NONE',  ( 16.56782317627811096, 0.008141063682853480823, -0.005492611183758445634 ) ) ;
#7200 = EDGE_CURVE ( 'NONE', #7133, #16692, #18087, .T. ) ;
#7201 = ADVANCED_FACE ( 'NONE', ( #13508 ), #5955, .F. ) ;
#7202 =( LENGTH_UNIT ( ) NAMED_UNIT ( * ) SI_UNIT ( .MILLI., .METRE. ) );
#7203 = CARTESIAN_POINT ( 'NONE',  ( 16.56679352167444819, 0.006618561353600086947, 0.006526964904752371663 ) ) ;
#7204 = DIRECTION ( 'NONE',  ( -1.000000000000000000, -0.000000000000000000, -0.000000000000000000 ) ) ;
#7205 = B_SPLINE_CURVE_WITH_KNOTS ( 'NONE', 3,
 ( #18743, #5465, #6914, #1260 ),
 .UNSPECIFIED., .F., .F.,
 ( 4, 4 ),
 ( 0.000000000000000000, 0.002004993803842804005 ),
 .UNSPECIFIED. ) ;
#7206 = AXIS2_PLACEMENT_3D ( 'NONE', #16877, #3781, #9610 ) ;
#7207 =( GEOMETRIC_REPRESENTATION_CONTEXT ( 3 ) GLOBAL_UNCERTAINTY_ASSIGNED_CONTEXT ( ( #5929 ) ) GLOBAL_UNIT_ASSIGNED_CONTEXT ( ( #1487, #45, #339 ) ) REPRESENTATION_CONTEXT ( 'NONE', 'WORKASPACE' ) );
#7208 = EDGE_CURVE ( 'NONE', #10123, #13902, #2493, .T. ) ;
#7209 = CARTESIAN_POINT ( 'NONE',  ( 3.950837973638677170, 13.10350451991849141, -6.316429227969337923 ) ) ;
#7210 = CARTESIAN_POINT ( 'NONE',  ( 2.002547531651519996, -11.75462648437098601, -4.532360870844453160 ) ) ;
#7211 = FACE_OUTER_BOUND ( 'NONE', #9431, .T. ) ;
#7212 = ORIENTED_EDGE ( 'NONE', *, *, #9685, .F. ) ;
#7213 = CARTESIAN_POINT ( 'NONE',  ( 0.3720661004400040439, -3.575426119359279564, 13.34435358167251984 ) ) ;
#7214 = FACE_OUTER_BOUND ( 'NONE', #14533, .T. ) ;
#7215 = ORIENTED_EDGE ( 'NONE', *, *, #2738, .F. ) ;
#7216 = EDGE_CURVE ( 'NONE', #8524, #13924, #5086, .T. ) ;
#7217 = ORIENTED_EDGE ( 'NONE', *, *, #8387, .T. ) ;
#7218 = CARTESIAN_POINT ( 'NONE',  ( 16.57778382496167424, 0.007244066302946777433, 0.01306626476309292149 ) ) ;
#7219 = EDGE_LOOP ( 'NONE', ( #7789, #16574, #6350, #16982 ) ) ;
#7220 = CARTESIAN_POINT ( 'NONE',  ( 0.4754618798421162973, -13.89949764182682124, -0.7484603771385882620 ) ) ;
#7221 = EDGE_LOOP ( 'NONE', ( #4487, #6537, #18328, #12753 ) ) ;
#7222 = AXIS2_PLACEMENT_3D ( 'NONE', #2085, #8740, #14289 ) ;
#7223 = DIRECTION ( 'NONE',  ( 0.7561779333270775005, -0.5081796452863246438, -0.4122479608995723299 ) ) ;
#7224 = CARTESIAN_POINT ( 'NONE',  ( 0.8740764193769881008, 5.211550415969331773, -13.31469591265785901 ) ) ;
#7225 = PRODUCT_DEFINITION_SHAPE ( 'NONE', 'NONE',  #6272 ) ;
#7226 = CARTESIAN_POINT ( 'NONE',  ( -2.749999999999997780, 3.367778697655218546E-16, 7.000000000000000000 ) ) ;
#7227 = CARTESIAN_POINT ( 'NONE',  ( 1.977436885027412439, 13.27782258182005748, -7.806953934146017460 ) ) ;
#7228 = CARTESIAN_POINT ( 'NONE',  ( 22.75000000000000000, 0.000000000000000000, 2.055000000000000160 ) ) ;
#7229 = CARTESIAN_POINT ( 'NONE',  ( 0.4862570985993252548, 10.79774104611373353, 8.769551628660776643 ) ) ;
#7230 = EDGE_CURVE ( 'NONE', #13316, #7194, #2883, .T. ) ;
#7231 = EDGE_LOOP ( 'NONE', ( #5136, #5586, #2383, #4823, #1059, #2826 ) ) ;
#7232 = B_SPLINE_CURVE_WITH_KNOTS ( 'NONE', 3,
 ( #7189, #11391, #17209, #2483, #14345, #9946 ),
 .UNSPECIFIED., .F., .F.,
 ( 4, 2, 4 ),
 ( 1.305552300251627978E-18, 0.001657017934710633541, 0.003314035869421265781 ),
 .UNSPECIFIED. ) ;
#7233 = AXIS2_PLACEMENT_3D ( 'NONE', #14144, #6893, #2567 ) ;
#7234 = VERTEX_POINT ( 'NONE', #35 ) ;
#7235 = VECTOR ( 'NONE', #6453, 1000.000000000000000 ) ;
#7236 = ADVANCED_FACE ( 'NONE', ( #11695 ), #17523, .F. ) ;
#7237 = EDGE_LOOP ( 'NONE', ( #1081, #1699, #12381, #7281 ) ) ;
#7238 = ORIENTED_EDGE ( 'NONE', *, *, #6908, .F. ) ;
#7239 = ORIENTED_EDGE ( 'NONE', *, *, #1979, .T. ) ;
#7240 =( BOUNDED_SURFACE ( )  B_SPLINE_SURFACE ( 3, 1, ( 
 ( #2433, #1005 ),
 ( #5576, #16975 ),
 ( #6843, #15441 ),
 ( #18674, #2352 ) ),
 .UNSPECIFIED., .F., .F., .T. ) 
 B_SPLINE_SURFACE_WITH_KNOTS ( ( 4, 4 ),
 ( 2, 2 ),
 ( 0.000000000000000000, 1.000000000000000000 ),
 ( 0.000000000000000000, 1.000000000000000000 ),
 .UNSPECIFIED. ) 
 GEOMETRIC_REPRESENTATION_ITEM ( )  RATIONAL_B_SPLINE_SURFACE ( (
 ( 1.000000000000000000, 1.000000000000000000),
 ( 0.9933953342250436691, 0.8357391271907733676),
 ( 0.9933953342250436691, 0.8357391271907733676),
 ( 1.000000000000000000, 1.000000000000000000) ) ) 
 REPRESENTATION_ITEM ( '' )  SURFACE ( )  );
#7241 = DIRECTION ( 'NONE',  ( 2.602085213965210642E-15, 0.000000000000000000, 1.000000000000000000 ) ) ;
#7242 = FACE_BOUND ( 'NONE', #13550, .T. ) ;
#7243 = CYLINDRICAL_SURFACE ( 'NONE', #14834, 1.000000000000000000 ) ;
#7244 = EDGE_LOOP ( 'NONE', ( #13551, #11769, #15161, #8726 ) ) ;
#7245 = CARTESIAN_POINT ( 'NONE',  ( 16.56753206892534891, -0.001421777558676013808, 0.009389754735542241854 ) ) ;
#7246 = AXIS2_PLACEMENT_3D ( 'NONE', #18856, #29, #7601 ) ;
#7247 = CARTESIAN_POINT ( 'NONE',  ( 3.950837973638677170, 6.316429227969654114, -13.10350451991833687 ) ) ;
#7248 = DIRECTION ( 'NONE',  ( 0.000000000000000000, -1.000000000000000000, 0.000000000000000000 ) ) ;
#7249 = CLOSED_SHELL ( 'NONE', ( #13576, #7332, #601, #8241, #851, #12848, #16673, #11406 ) ) ;
#7250 = FACE_OUTER_BOUND ( 'NONE', #13130, .T. ) ;
#7251 = CARTESIAN_POINT ( 'NONE',  ( 1.977228804422749064, -1.488378900182820264, -15.33060379559159259 ) ) ;
#7252 = CARTESIAN_POINT ( 'NONE',  ( 2.002547531651519996, 12.17374746633582561, -3.242439124566524278 ) ) ;
#7253 = CARTESIAN_POINT ( 'NONE',  ( 0.8740779401506997282, 9.070947476926598085, 11.05257166392028267 ) ) ;
#7254 = DIRECTION ( 'NONE',  ( 0.000000000000000000, 0.000000000000000000, -1.000000000000000000 ) ) ;
#7255 = CARTESIAN_POINT ( 'NONE',  ( 3.512766787570778870, -6.535475144496882827, -13.55823433651953636 ) ) ;
#7256 = ORIENTED_EDGE ( 'NONE', *, *, #2547, .T. ) ;
#7257 = ORIENTED_EDGE ( 'NONE', *, *, #3891, .T. ) ;
#7258 = ADVANCED_FACE ( 'NONE', ( #10944 ), #13806, .T. ) ;
#7259 = EDGE_CURVE ( 'NONE', #16918, #1375, #2147, .T. ) ;
#7260 = EDGE_CURVE ( 'NONE', #349, #13704, #10457, .T. ) ;
#7261 = VERTEX_POINT ( 'NONE', #707 ) ;
#7262 = EDGE_LOOP ( 'NONE', ( #11071, #6519, #16032, #6583 ) ) ;
#7263 = CARTESIAN_POINT ( 'NONE',  ( 1.562796894703937678, 0.000000000000000000, 0.000000000000000000 ) ) ;
#7264 = ORIENTED_EDGE ( 'NONE', *, *, #9862, .T. ) ;
#7265 = CARTESIAN_POINT ( 'NONE',  ( 1.861706995891666105, 3.332865258614144732, -12.00328602385076593 ) ) ;
#7266 = CARTESIAN_POINT ( 'NONE',  ( 1.846524061778021419, 11.71897913237549105, 4.180439405448364454 ) ) ;
#7267 = CARTESIAN_POINT ( 'NONE',  ( 0.3720661004400040439, 7.524064345033631973, -11.58636699658207370 ) ) ;
#7268 = FACE_OUTER_BOUND ( 'NONE', #11369, .T. ) ;
#7269 = ORIENTED_EDGE ( 'NONE', *, *, #16992, .F. ) ;
#7270 = DIRECTION ( 'NONE',  ( -0.000000000000000000, -0.000000000000000000, 1.000000000000000000 ) ) ;
#7271 = AXIS2_PLACEMENT_3D ( 'NONE', #10569, #437, #6266 ) ;
#7272 = DIRECTION ( 'NONE',  ( 1.000000000000000000, 0.000000000000000000, -0.000000000000000000 ) ) ;
#7273 = CARTESIAN_POINT ( 'NONE',  ( 0.3137051932979792457, -13.73004976592202375, 0.4596302728639276580 ) ) ;
#7274 = CARTESIAN_POINT ( 'NONE',  ( 0.3095370825347224519, 8.444334731364007141, 10.84046130709061373 ) ) ;
#7275 = CARTESIAN_POINT ( 'NONE',  ( 1.846955891736117517, 11.91257079808168839, 3.593597880662386945 ) ) ;
#7276 = CARTESIAN_POINT ( 'NONE',  ( 2.697797270744668463, 0.9169917281809109033, -13.26309265156976203 ) ) ;
#7277 =( BOUNDED_SURFACE ( )  B_SPLINE_SURFACE ( 3, 1, ( 
 ( #15190, #13833 ),
 ( #15359, #13663 ),
 ( #10795, #930 ),
 ( #16618, #9358 ) ),
 .UNSPECIFIED., .F., .F., .F. ) 
 B_SPLINE_SURFACE_WITH_KNOTS ( ( 4, 4 ),
 ( 2, 2 ),
 ( 0.000000000000000000, 1.000000000000000000 ),
 ( 0.000000000000000000, 1.000000000000000000 ),
 .UNSPECIFIED. ) 
 GEOMETRIC_REPRESENTATION_ITEM ( )  RATIONAL_B_SPLINE_SURFACE ( (
 ( 1.000000000000000000, 1.000000000000000000),
 ( 0.7792777138730158093, 0.9689936506012928330),
 ( 0.7792777138730158093, 0.9689936506012928330),
 ( 1.000000000000000000, 1.000000000000000000) ) ) 
 REPRESENTATION_ITEM ( '' )  SURFACE ( )  );
#7278 = DIRECTION ( 'NONE',  ( -1.000000000000000000, -0.000000000000000000, -0.000000000000000000 ) ) ;
#7279 = VERTEX_POINT ( 'NONE', #13979 ) ;
#7281 = ORIENTED_EDGE ( 'NONE', *, *, #4558, .T. ) ;
#7280 = CARTESIAN_POINT ( 'NONE',  ( 1.847421816787903071, 0.02876707915197697710, -12.44300551404155364 ) ) ;
#7282 = EDGE_CURVE ( 'NONE', #1657, #767, #4174, .T. ) ;
#7283 = CARTESIAN_POINT ( 'NONE',  ( 16.56822296793089322, -0.008619100080558715279, 0.005339139727952894703 ) ) ;
#7284 = ADVANCED_FACE ( 'NONE', ( #16491 ), #6540, .F. ) ;
#7285 = ADVANCED_FACE ( 'NONE', ( #8164 ), #15414, .T. ) ;
#7286 = DIRECTION ( 'NONE',  ( 0.000000000000000000, -1.000000000000000000, 0.000000000000000000 ) ) ;
#7287 = EDGE_CURVE ( 'NONE', #7021, #4376, #9005, .T. ) ;
#7288 = ORIENTED_EDGE ( 'NONE', *, *, #17295, .F. ) ;
#7289 = DIRECTION ( 'NONE',  ( -0.000000000000000000, -0.000000000000000000, -1.000000000000000000 ) ) ;
#7290 = DIRECTION ( 'NONE',  ( 0.000000000000000000, 0.000000000000000000, -1.000000000000000000 ) ) ;
#7291 = EDGE_LOOP ( 'NONE', ( #16933, #12009, #4431, #5661 ) ) ;
#7292 = DIRECTION ( 'NONE',  ( 0.000000000000000000, 0.000000000000000000, 1.000000000000000000 ) ) ;
#7293 = LINE ( 'NONE', #5836, #14620 ) ;
#7294 = B_SPLINE_CURVE_WITH_KNOTS ( 'NONE', 3,
 ( #14542, #17413, #7098, #2494, #17315, #4233 ),
 .UNSPECIFIED., .F., .F.,
 ( 4, 2, 4 ),
 ( 0.000000000000000000, 0.001656992708821696143, 0.003313985417643392287 ),
 .UNSPECIFIED. ) ;
#7295 = CARTESIAN_POINT ( 'NONE',  ( 0.3142011359265320380, -3.879426116491784260, 13.17934269988456819 ) ) ;
#7296 = CARTESIAN_POINT ( 'NONE',  ( 0.3939822652208137543, 11.57634296752778802, -7.545099438011897419 ) ) ;
#7297 = CONTEXT_DEPENDENT_SHAPE_REPRESENTATION ( #14020, #4954 ) ;
#7298 =( NAMED_UNIT ( * ) PLANE_ANGLE_UNIT ( ) SI_UNIT ( $, .RADIAN. ) );
#7299 = PLANE ( 'NONE',  #4988 ) ;
#7300 = CARTESIAN_POINT ( 'NONE',  ( 0.3137051932979809665, -13.20008686438108647, 3.805684345189735307 ) ) ;
#7301 = CARTESIAN_POINT ( 'NONE',  ( 16.56872352241294521, 0.004564908236400220913, 0.009382111268606271176 ) ) ;
#7302 = CARTESIAN_POINT ( 'NONE',  ( 16.56679352167444819, 0.004162264567718796174, -0.008311568981097996328 ) ) ;
#7303 = DIRECTION ( 'NONE',  ( -1.000000000000000000, 0.000000000000000000, -0.000000000000000000 ) ) ;
#7304 = ORIENTED_EDGE ( 'NONE', *, *, #16141, .F. ) ;
#7305 = DIRECTION ( 'NONE',  ( 0.000000000000000000, 0.000000000000000000, 1.000000000000000000 ) ) ;
#7306 = DIRECTION ( 'NONE',  ( -1.000000000000000000, 0.000000000000000000, 0.000000000000000000 ) ) ;
#7307 = ORIENTED_EDGE ( 'NONE', *, *, #2528, .T. ) ;
#7308 = ADVANCED_FACE ( 'NONE', ( #15039 ), #17110, .F. ) ;
#7309 = ORIENTED_EDGE ( 'NONE', *, *, #2400, .F. ) ;
#7310 = CARTESIAN_POINT ( 'NONE',  ( 16.56872352241294521, 0.007240717549633990044, -0.007512283835805476720 ) ) ;
#7311 = EDGE_CURVE ( 'NONE', #3395, #10485, #5317, .T. ) ;
#7312 = ORIENTED_EDGE ( 'NONE', *, *, #2827, .T. ) ;
#7313 = DIRECTION ( 'NONE',  ( -1.000000000000000000, -0.000000000000000000, -0.000000000000000000 ) ) ;
#7314 = VECTOR ( 'NONE', #16851, 1000.000000000000000 ) ;
#7315 = MECHANICAL_DESIGN_GEOMETRIC_PRESENTATION_REPRESENTATION (  '', ( #5469 ), #4569 ) ;
#7316 = ORIENTED_EDGE ( 'NONE', *, *, #14797, .F. ) ;
#7317 = CARTESIAN_POINT ( 'NONE',  ( 1.846613052777650976, 9.862487290071108248, -7.585914669018062106 ) ) ;
#7318 = CARTESIAN_POINT ( 'NONE',  ( 0.8740779401506997282, 9.070947476926598085, 11.05257166392028267 ) ) ;
#7319 = CARTESIAN_POINT ( 'NONE',  ( 16.58200780006414732, 0.004047297414159048250, -0.01041078477704050417 ) ) ;
#7320 = AXIS2_PLACEMENT_3D ( 'NONE', #16023, #14590, #70 ) ;
#7321 = LINE ( 'NONE', #6166, #17868 ) ;
#7322 = DIRECTION ( 'NONE',  ( -1.913297951445007622E-16, 1.000000000000000000, 0.000000000000000000 ) ) ;
#7323 = CARTESIAN_POINT ( 'NONE',  ( 2.320520222536938348, -1.795797593768547085, 15.64520721754664123 ) ) ;
#7324 = CARTESIAN_POINT ( 'NONE',  ( 5.000000000000000000, 6.123233995736766282E-16, 8.000000000000000000 ) ) ;
#7325 = ORIENTED_EDGE ( 'NONE', *, *, #2865, .F. ) ;
#7326 = ADVANCED_FACE ( 'NONE', ( #1957 ), #7794, .F. ) ;
#7327 = FACE_OUTER_BOUND ( 'NONE', #9673, .T. ) ;
#7328 = CARTESIAN_POINT ( 'NONE',  ( 16.57210152137263393, 0.008007331252333427934, -0.01214401161737626612 ) ) ;
#7329 = ORIENTED_EDGE ( 'NONE', *, *, #12794, .T. ) ;
#7330 = B_SPLINE_CURVE_WITH_KNOTS ( 'NONE', 3,
 ( #3304, #1789, #354, #6183, #10585, #17950 ),
 .UNSPECIFIED., .F., .F.,
 ( 4, 2, 4 ),
 ( 0.000000000000000000, 0.0001828790815886945087, 0.0003657581631773890174 ),
 .UNSPECIFIED. ) ;
#7331 = DIRECTION ( 'NONE',  ( 0.000000000000000000, 0.000000000000000000, -1.000000000000000000 ) ) ;
#7332 = ADVANCED_FACE ( 'NONE', ( #15316 ), #12653, .T. ) ;
#7333 = B_SPLINE_CURVE_WITH_KNOTS ( 'NONE', 3,
 ( #18165, #1728, #3441, #9470, #10812, #595 ),
 .UNSPECIFIED., .F., .F.,
 ( 4, 2, 4 ),
 ( 3.436766974507050665E-17, 0.0001825746017570568534, 0.0003651492035140793376 ),
 .UNSPECIFIED. ) ;
#7334 = ORIENTED_EDGE ( 'NONE', *, *, #2969, .F. ) ;
#7335 = ORIENTED_EDGE ( 'NONE', *, *, #9135, .F. ) ;
#7336 = ORIENTED_EDGE ( 'NONE', *, *, #5050, .F. ) ;
#7337 = ORIENTED_EDGE ( 'NONE', *, *, #18211, .F. ) ;
#7338 = B_SPLINE_CURVE_WITH_KNOTS ( 'NONE', 3,
 ( #5034, #14978, #9440, #12125, #7733, #17958 ),
 .UNSPECIFIED., .F., .F.,
 ( 4, 2, 4 ),
 ( 0.000000000000000000, 0.001657017934709840989, 0.003314035869419681979 ),
 .UNSPECIFIED. ) ;
#7339 = CARTESIAN_POINT ( 'NONE',  ( 8.522092701127531811, -2.505958102592667824, 6.489356537178181838 ) ) ;
#7340 = CARTESIAN_POINT ( 'NONE',  ( 3.950837973638676281, 6.316429227969464932, 13.10350451991842569 ) ) ;
#7341 = DIRECTION ( 'NONE',  ( 2.891205793294679312E-16, 1.000000000000000000, 0.000000000000000000 ) ) ;
#7342 = ORIENTED_EDGE ( 'NONE', *, *, #18030, .F. ) ;
#7343 = PLANE ( 'NONE',  #10840 ) ;
#7344 = DIRECTION ( 'NONE',  ( 0.7561779333270775005, -0.5491072561318390832, 0.3559159372837255031 ) ) ;
#7345 = CARTESIAN_POINT ( 'NONE',  ( 1.560000000000000053, 0.000000000000000000, 2.999999999999998668 ) ) ;
#7346 = CARTESIAN_POINT ( 'NONE',  ( 2.002547531651519996, 6.845637710436341727, -10.57595306287284842 ) ) ;
#7347 = CARTESIAN_POINT ( 'NONE',  ( 8.522092701127531811, 0.3779863304872196350, -6.946128462138591253 ) ) ;
#7348 = EDGE_CURVE ( 'NONE', #348, #14985, #16578, .T. ) ;
#7349 = PLANE ( 'NONE',  #13603 ) ;
#7350 = CARTESIAN_POINT ( 'NONE',  ( 0.3720661004400040439, -11.58636699658209679, -7.524064345033593781 ) ) ;
#7351 = DIRECTION ( 'NONE',  ( -1.000000000000000000, 0.000000000000000000, 0.000000000000000000 ) ) ;
#7352 = CARTESIAN_POINT ( 'NONE',  ( 0.3148213771069373057, 4.463459503829174224, -12.99360322443197724 ) ) ;
#7353 = ORIENTED_EDGE ( 'NONE', *, *, #17360, .F. ) ;
#7354 = EDGE_CURVE ( 'NONE', #15939, #9014, #6358, .T. ) ;
#7355 =( BOUNDED_SURFACE ( )  B_SPLINE_SURFACE ( 3, 1, ( 
 ( #2271, #15729 ),
 ( #5416, #9627 ),
 ( #8120, #12862 ),
 ( #5589, #6772 ) ),
 .UNSPECIFIED., .F., .F., .T. ) 
 B_SPLINE_SURFACE_WITH_KNOTS ( ( 4, 4 ),
 ( 2, 2 ),
 ( 0.000000000000000000, 1.000000000000000000 ),
 ( 0.000000000000000000, 1.000000000000000000 ),
 .UNSPECIFIED. ) 
 GEOMETRIC_REPRESENTATION_ITEM ( )  RATIONAL_B_SPLINE_SURFACE ( (
 ( 1.000000000000000000, 1.000000000000000000),
 ( 0.9933953342250436691, 0.8357391271907733676),
 ( 0.9933953342250436691, 0.8357391271907733676),
 ( 1.000000000000000000, 1.000000000000000000) ) ) 
 REPRESENTATION_ITEM ( '' )  SURFACE ( )  );
#7356 = ORIENTED_EDGE ( 'NONE', *, *, #12769, .T. ) ;
#7357 = ORIENTED_EDGE ( 'NONE', *, *, #8965, .F. ) ;
#7358 = ORIENTED_EDGE ( 'NONE', *, *, #12308, .T. ) ;
#7359 = CARTESIAN_POINT ( 'NONE',  ( 16.56822296793089322, 0.008619100080558677116, -0.005339139727952955418 ) ) ;
#7360 = ORIENTED_EDGE ( 'NONE', *, *, #4718, .T. ) ;
#7361 = CARTESIAN_POINT ( 'NONE',  ( 1.845756295923353996, 3.386818134580228179, -11.97166802574122890 ) ) ;
#7362 = DIRECTION ( 'NONE',  ( -1.000000000000000000, -0.000000000000000000, -0.000000000000000000 ) ) ;
#7363 = CARTESIAN_POINT ( 'NONE',  ( 8.438534575730034959, -3.845978796786076348, 5.688336279099031501 ) ) ;
#7364 = DIRECTION ( 'NONE',  ( -0.000000000000000000, -0.000000000000000000, 1.000000000000000000 ) ) ;
#7365 = ORIENTED_EDGE ( 'NONE', *, *, #7703, .T. ) ;
#7366 = FACE_BOUND ( 'NONE', #6245, .T. ) ;
#7367 = CARTESIAN_POINT ( 'NONE',  ( 0.3148213771069355293, -4.026433757158891957, -13.13560149728604998 ) ) ;
#7368 = B_SPLINE_CURVE_WITH_KNOTS ( 'NONE', 3,
 ( #14441, #11394, #9949, #15503, #12911, #6812 ),
 .UNSPECIFIED., .F., .F.,
 ( 4, 2, 4 ),
 ( 4.192373019364431701E-17, 0.0002014099069817294621, 0.0004028198139634169657 ),
 .UNSPECIFIED. ) ;
#7369 = DIRECTION ( 'NONE',  ( 0.000000000000000000, 0.000000000000000000, -1.000000000000000000 ) ) ;
#7370 = ADVANCED_FACE ( 'NONE', ( #3567 ), #10010, .F. ) ;
#7371 = DIRECTION ( 'NONE',  ( 0.000000000000000000, -0.000000000000000000, 1.000000000000000000 ) ) ;
#7372 = EDGE_CURVE ( 'NONE', #6541, #13630, #1922, .T. ) ;
#7373 = CARTESIAN_POINT ( 'NONE',  ( 0.3142014840576536350, 12.94260032291128759, 4.608051180496968158 ) ) ;
#7374 = ORIENTED_EDGE ( 'NONE', *, *, #625, .F. ) ;
#7375 = ORIENTED_EDGE ( 'NONE', *, *, #18179, .F. ) ;
#7376 = CARTESIAN_POINT ( 'NONE',  ( 1.847380140988740260, 7.224522571381473135, -10.13114603776188893 ) ) ;
#7378 = VERTEX_POINT ( 'NONE', #5459 ) ;
#7377 = CARTESIAN_POINT ( 'NONE',  ( 1.560000000000000053, -0.8660254037844384856, -1.500000000000000000 ) ) ;
#7379 = CARTESIAN_POINT ( 'NONE',  ( 0.3137051932979792457, 8.442169467527008919, -10.83767969834794087 ) ) ;
#7380 = CARTESIAN_POINT ( 'NONE',  ( 0.4754618798421162973, 13.89949764182682657, -0.7484603771384912285 ) ) ;
#7381 = VERTEX_POINT ( 'NONE', #17309 ) ;
#7382 = CARTESIAN_POINT ( 'NONE',  ( 0.3939875929385642239, -0.7003304234512184312, -13.80036004410494854 ) ) ;
#7383 = CARTESIAN_POINT ( 'NONE',  ( 1.715145640900883395, -6.797472175340068645, -12.00000001230414348 ) ) ;
#7384 = ORIENTED_EDGE ( 'NONE', *, *, #8086, .F. ) ;
#7385 = CARTESIAN_POINT ( 'NONE',  ( 1.846138399168762101, -4.238866729160323032, -11.69739621335926394 ) ) ;
#7386 = LINE ( 'NONE', #13200, #16157 ) ;
#7387 = LINE ( 'NONE', #3054, #5757 ) ;
#7388 = CARTESIAN_POINT ( 'NONE',  ( 0.000000000000000000, 0.000000000000000000, 8.000000000000000000 ) ) ;
#7389 = EDGE_CURVE ( 'NONE', #14913, #1370, #7368, .T. ) ;
#7390 = EDGE_CURVE ( 'NONE', #11620, #8960, #1433, .T. ) ;
#7391 = EDGE_CURVE ( 'NONE', #4602, #18903, #10789, .T. ) ;
#7392 = VECTOR ( 'NONE', #13786, 1000.000000000000000 ) ;
#7393 =( NAMED_UNIT ( * ) SI_UNIT ( $, .STERADIAN. ) SOLID_ANGLE_UNIT ( ) );
#7394 = DIRECTION ( 'NONE',  ( 0.000000000000000000, -0.8660254037844384856, -0.5000000000000004441 ) ) ;
#7395 = CARTESIAN_POINT ( 'NONE',  ( 16.57778382496167424, 0.001819584982831899374, -0.01482878558584570412 ) ) ;
#7396 = CARTESIAN_POINT ( 'NONE',  ( 1.861706995891675653, 0.5394761475745838419, 12.44571539481144207 ) ) ;
#7397 = CARTESIAN_POINT ( 'NONE',  ( 0.3170788640506441158, -7.952793437297652090, 11.20690911610900997 ) ) ;
#7398 = CARTESIAN_POINT ( 'NONE',  ( 1.959212340397962882, -12.53706137681889210, -0.6675998551413099280 ) ) ;
#7399 = ORIENTED_EDGE ( 'NONE', *, *, #11488, .F. ) ;
#7400 = CARTESIAN_POINT ( 'NONE',  ( 1.845756295923359547, 4.296776483139476355, 11.67600463554274626 ) ) ;
#7401 = CARTESIAN_POINT ( 'NONE',  ( 3.950837973638668288, 0.000000000000000000, 0.000000000000000000 ) ) ;
#7402 = B_SPLINE_CURVE_WITH_KNOTS ( 'NONE', 3,
 ( #16705, #9617, #12128, #3789, #652, #3415 ),
 .UNSPECIFIED., .F., .F.,
 ( 4, 2, 4 ),
 ( 0.000000000000000000, 0.001500839035891550054, 0.003001678071783100109 ),
 .UNSPECIFIED. ) ;
#7403 = ORIENTED_EDGE ( 'NONE', *, *, #16309, .F. ) ;
#7404 = ORIENTED_EDGE ( 'NONE', *, *, #5570, .T. ) ;
#7405 = CARTESIAN_POINT ( 'NONE',  ( 0.3095370825347224519, -7.700448427571953580, 11.38092634279625770 ) ) ;
#7406 = ORIENTED_EDGE ( 'NONE', *, *, #5834, .T. ) ;
#7407 = CARTESIAN_POINT ( 'NONE',  ( 1.959212340397945562, 3.239239832449027467, 12.12975361829676579 ) ) ;
#7408 = AXIS2_PLACEMENT_3D ( 'NONE', #10264, #7313, #6253 ) ;
#7409 = ORIENTED_EDGE ( 'NONE', *, *, #5610, .T. ) ;
#7410 = CARTESIAN_POINT ( 'NONE',  ( 2.705023505549866147, 7.115606223895331262, -11.23800170568049062 ) ) ;
#7411 = B_SPLINE_CURVE_WITH_KNOTS ( 'NONE', 3,
 ( #2914, #18794, #10299, #18695, #15738, #7150 ),
 .UNSPECIFIED., .F., .F.,
 ( 4, 2, 4 ),
 ( 0.000000000000000000, 0.0001828790815886944003, 0.0003657581631773888006 ),
 .UNSPECIFIED. ) ;
#7412 = CARTESIAN_POINT ( 'NONE',  ( 1.254009781011257374, 12.44229282923036628, 7.789615163754328719 ) ) ;
#7413 = CARTESIAN_POINT ( 'NONE',  ( 16.57210152137263393, -0.01453130299868521901, -0.0006600038696347544425 ) ) ;
#7414 = CARTESIAN_POINT ( 'NONE',  ( -199.9999999999999716, -5.000000000000024869, -2.000000000000000000 ) ) ;
#7415 = CARTESIAN_POINT ( 'NONE',  ( 16.56822296793089322, -0.009385634690641594599, -0.003834730849370937035 ) ) ;
#7416 = CARTESIAN_POINT ( 'NONE',  ( -199.9999999999999716, 4.999999999999973355, 11.00000000000000000 ) ) ;
#7417 = SURFACE_STYLE_USAGE ( .BOTH. , #11707 ) ;
#7418 = CARTESIAN_POINT ( 'NONE',  ( 0.4862570985993235340, -3.580942890621579444, -13.44146924561384537 ) ) ;
#7419 = CARTESIAN_POINT ( 'NONE',  ( -194.9999999999999716, 9.999999999999973355, 6.000000000000000000 ) ) ;
#7420 = EDGE_CURVE ( 'NONE', #3596, #7837, #10044, .T. ) ;
#7421 = ADVANCED_FACE ( 'NONE', ( #14158 ), #10847, .T. ) ;
#7422 = DIRECTION ( 'NONE',  ( 2.891205793294679312E-16, -1.000000000000000000, -0.000000000000000000 ) ) ;
#7423 = CARTESIAN_POINT ( 'NONE',  ( 16.56872352241294521, 0.009207754980064196751, -0.004907101719995712874 ) ) ;
#7424 = CARTESIAN_POINT ( 'NONE',  ( 1.847034903785822690, -11.90269060117936739, 3.625649561595261083 ) ) ;
#7425 = ORIENTED_EDGE ( 'NONE', *, *, #1125, .T. ) ;
#7426 = ADVANCED_FACE ( 'NONE', ( #18840 ), #2404, .F. ) ;
#7427 = AXIS2_PLACEMENT_3D ( 'NONE', #11524, #12849, #2710 ) ;
#7428 = ORIENTED_EDGE ( 'NONE', *, *, #6341, .F. ) ;
#7429 = ORIENTED_EDGE ( 'NONE', *, *, #17630, .T. ) ;
#7430 = ORIENTED_EDGE ( 'NONE', *, *, #4096, .T. ) ;
#7431 = CARTESIAN_POINT ( 'NONE',  ( -1.979226605763932723, -19.99999999999999645, 6.000000000000000000 ) ) ;
#7432 = PLANE ( 'NONE',  #16650 ) ;
#7433 = CARTESIAN_POINT ( 'NONE',  ( 16.56872352241294521, 0.009207754980064196751, -0.004907101719995712874 ) ) ;
#7434 = ORIENTED_EDGE ( 'NONE', *, *, #6830, .F. ) ;
#7435 = CARTESIAN_POINT ( 'NONE',  ( 20.00000000000000711, -19.99999999999999645, 6.000000000000000000 ) ) ;
#7436 = DIRECTION ( 'NONE',  ( 1.000000000000000000, -0.000000000000000000, 2.775557561562891351E-15 ) ) ;
#7437 = CARTESIAN_POINT ( 'NONE',  ( 0.4862570985993235340, 8.769551628660890330, -10.79774104611363761 ) ) ;
#7438 = CARTESIAN_POINT ( 'NONE',  ( 1.342453679581834924, -3.649820028552632767, -14.34050741580210619 ) ) ;
#7439 = CARTESIAN_POINT ( 'NONE',  ( 0.3142014840576498047, 7.762239086932858356, 11.33546131209465102 ) ) ;
#7440 = EDGE_CURVE ( 'NONE', #12470, #11533, #14660, .T. ) ;
#7441 = TOROIDAL_SURFACE ( 'NONE', #3773, 5.000000000000005329, 5.000000000000000000 ) ;
#7442 = CARTESIAN_POINT ( 'NONE',  ( 1.846138399168762101, 11.95493567637855392, -3.446241763652874379 ) ) ;
#7443 = CARTESIAN_POINT ( 'NONE',  ( 1.846138399168762989, 9.815003036200414144, 7.646096044339929954 ) ) ;
#7444 = ADVANCED_FACE ( 'NONE', ( #18458 ), #4739, .T. ) ;
#7445 = DIRECTION ( 'NONE',  ( -0.7635533937278216055, 0.6453904417649387604, -0.02138673900302117195 ) ) ;
#7446 = ADVANCED_FACE ( 'NONE', ( #2487 ), #4128, .F. ) ;
#7447 = CARTESIAN_POINT ( 'NONE',  ( 0.3142011359265305948, -8.382042760265827397, -10.88514493056451471 ) ) ;
#7448 = EDGE_LOOP ( 'NONE', ( #14016, #12356, #13851, #13700 ) ) ;
#7449 = EDGE_LOOP ( 'NONE', ( #10499, #15432, #2165, #912 ) ) ;
#7450 = VERTEX_POINT ( 'NONE', #15589 ) ;
#7451 = ORIENTED_EDGE ( 'NONE', *, *, #375, .F. ) ;
#7452 = CARTESIAN_POINT ( 'NONE',  ( 3.950837973638677170, 13.10350451991849141, -6.316429227969337923 ) ) ;
#7453 = ADVANCED_FACE ( 'NONE', ( #8523 ), #14348, .T. ) ;
#7454 = VERTEX_POINT ( 'NONE', #18556 ) ;
#7455 = CARTESIAN_POINT ( 'NONE',  ( 2.353870697619110608, -10.00946331859657334, -8.216087327473042379 ) ) ;
#7456 = VECTOR ( 'NONE', #7344, 1000.000000000000114 ) ;
#7457 = AXIS2_PLACEMENT_3D ( 'NONE', #12594, #15839, #18520 ) ;
#7458 = CARTESIAN_POINT ( 'NONE',  ( -5.000000000000000000, 20.00000000000000000, 4.000000000000000000 ) ) ;
#7459 = LINE ( 'NONE', #11846, #8088 ) ;
#7460 = CARTESIAN_POINT ( 'NONE',  ( 0.000000000000000000, 0.000000000000000000, -12.00000000000000000 ) ) ;
#7461 = ORIENTED_EDGE ( 'NONE', *, *, #11992, .T. ) ;
#7462 = CARTESIAN_POINT ( 'NONE',  ( -0.6293707761309729198, 7.500000000000000000, -14.32724244806440161 ) ) ;
#7463 = CARTESIAN_POINT ( 'NONE',  ( 1.321128355694181398E-14, -9.013167318348349610, 25.01316734529530095 ) ) ;
#7464 = CARTESIAN_POINT ( 'NONE',  ( 2.636624412717099908, 14.46769361191384817, -6.973567714910368309 ) ) ;
#7465 =( NAMED_UNIT ( * ) SI_UNIT ( $, .STERADIAN. ) SOLID_ANGLE_UNIT ( ) );
#7466 = PRODUCT ( 'BR-823', 'BR-823', '', ( #8351 ) ) ;
#7467 = CARTESIAN_POINT ( 'NONE',  ( 16.56753206892534891, -0.006760771273035160941, 0.006669401563385170262 ) ) ;
#7468 = ORIENTED_EDGE ( 'NONE', *, *, #17300, .F. ) ;
#7469 = AXIS2_PLACEMENT_3D ( 'NONE', #5556, #17227, #10156 ) ;
#7470 = CARTESIAN_POINT ( 'NONE',  ( 2.636624412714994037, -14.46769361191274328, -6.973567714907344950 ) ) ;
#7472 = ORIENTED_EDGE ( 'NONE', *, *, #11876, .T. ) ;
#7471 = CARTESIAN_POINT ( 'NONE',  ( 2.636624412716045196, 11.10302021257998994, -11.60464335004042447 ) ) ;
#7473 = CARTESIAN_POINT ( 'NONE',  ( 0.3150686449036038672, 7.951193823202562072, -11.20479228691389118 ) ) ;
#7474 = ADVANCED_FACE ( 'NONE', ( #17801 ), #208, .T. ) ;
#7475 = EDGE_CURVE ( 'NONE', #13012, #16693, #461, .T. ) ;
#7476 = VERTEX_POINT ( 'NONE', #4702 ) ;
#7477 = CARTESIAN_POINT ( 'NONE',  ( -30.00000000000000711, 20.00000000000000000, 3.000000000000000000 ) ) ;
#7478 = UNCERTAINTY_MEASURE_WITH_UNIT (LENGTH_MEASURE( 1.000000000000000082E-05 ), #15328, 'distance_accuracy_value', 'NONE');
#7479 = CARTESIAN_POINT ( 'NONE',  ( 4.196046169205040144, -7.500000000000000888, -16.53685941778015689 ) ) ;
#7480 = EDGE_LOOP ( 'NONE', ( #16037, #10474, #17253, #2274 ) ) ;
#7481 = PLANE ( 'NONE',  #16083 ) ;
#7482 = VECTOR ( 'NONE', #17557, 1000.000000000000114 ) ;
#7483 = CARTESIAN_POINT ( 'NONE',  ( 2.002547531651519996, 11.75462648437101976, 4.532360870844369671 ) ) ;
#7484 = CIRCLE ( 'NONE', #8695, 11.50000000000000178 ) ;
#7485 = DIRECTION ( 'NONE',  ( 1.000000000000000000, 0.000000000000000000, 0.000000000000000000 ) ) ;
#7486 = VECTOR ( 'NONE', #621, 1000.000000000000227 ) ;
#7487 = ORIENTED_EDGE ( 'NONE', *, *, #16581, .F. ) ;
#7488 = CARTESIAN_POINT ( 'NONE',  ( 0.3095370825347224519, -8.444334731363925428, -10.84046130709067768 ) ) ;
#7489 = DIRECTION ( 'NONE',  ( 0.000000000000000000, 0.000000000000000000, 1.000000000000000000 ) ) ;
#7490 = CARTESIAN_POINT ( 'NONE',  ( 2.636624412714236865, 0.000000000000000000, 0.000000000000000000 ) ) ;
#7491 = CARTESIAN_POINT ( 'NONE',  ( 1.342453679581834924, 0.9602753779830727199, 14.76648944001039787 ) ) ;
#7492 = CARTESIAN_POINT ( 'NONE',  ( 0.4754618798421167414, 13.45049478164064638, -3.583352865732531534 ) ) ;
#7493 = AXIS2_PLACEMENT_3D ( 'NONE', #12365, #15508, #6817 ) ;
#7494 = ORIENTED_EDGE ( 'NONE', *, *, #625, .T. ) ;
#7495 = CARTESIAN_POINT ( 'NONE',  ( 0.3137051932979757485, -7.698472063774552510, 11.37800749014128421 ) ) ;
#7496 = CARTESIAN_POINT ( 'NONE',  ( 0.3137051932979792457, -13.73004976592202375, 0.4596302728639276580 ) ) ;
#7497 = AXIS2_PLACEMENT_3D ( 'NONE', #12478, #16521, #6289 ) ;
#7498 = ORIENTED_EDGE ( 'NONE', *, *, #404, .T. ) ;
#7499 = ADVANCED_FACE ( 'NONE', ( #17502 ), #23, .T. ) ;
#7500 = ADVANCED_FACE ( 'NONE', ( #6706 ), #4412, .T. ) ;
#7501 = EDGE_CURVE ( 'NONE', #16313, #7003, #8680, .T. ) ;
#7502 = VERTEX_POINT ( 'NONE', #15754 ) ;
#7503 = CARTESIAN_POINT ( 'NONE',  ( 1.846822687350018866, -0.2922081769261017925, 12.43915556955403723 ) ) ;
#7504 = EDGE_LOOP ( 'NONE', ( #7472, #17912, #4680, #10601 ) ) ;
#7505 = DIRECTION ( 'NONE',  ( -0.000000000000000000, -0.000000000000000000, 1.000000000000000000 ) ) ;
#7506 = VERTEX_POINT ( 'NONE', #14052 ) ;
#7507 = CARTESIAN_POINT ( 'NONE',  ( 1.847372867223022519, 10.12831093686732586, -7.228345833872643844 ) ) ;
#7508 = CARTESIAN_POINT ( 'NONE',  ( 16.56872352241294521, 0.007240717549633888563, 0.007512283835804339609 ) ) ;
#7509 = CARTESIAN_POINT ( 'NONE',  ( 1.254009781011254487, 14.64464726212552037, -1.011465182607978130 ) ) ;
#7510 = CARTESIAN_POINT ( 'NONE',  ( 0.3132642857406529591, -8.495623922778147374, 10.79548167658031588 ) ) ;
#7511 = UNCERTAINTY_MEASURE_WITH_UNIT (LENGTH_MEASURE( 1.000000000000000082E-05 ), #607, 'distance_accuracy_value', 'NONE');
#7512 = VECTOR ( 'NONE', #14192, 1000.000000000000114 ) ;
#7513 = CARTESIAN_POINT ( 'NONE',  ( 0.3137051932979757485, -7.698472063774552510, 11.37800749014128421 ) ) ;
#7514 = CARTESIAN_POINT ( 'NONE',  ( 2.002547531651519996, 12.57989064830759496, -0.6781519942172177240 ) ) ;
#7515 = AXIS2_PLACEMENT_3D ( 'NONE', #6314, #13182, #7662 ) ;
#7516 = EDGE_CURVE ( 'NONE', #9395, #18705, #7796, .T. ) ;
#7517 = CARTESIAN_POINT ( 'NONE',  ( -59.99999999999997158, -10.00000000000000888, 6.000000000000000000 ) ) ;
#7518 = CARTESIAN_POINT ( 'NONE',  ( 1.846138399168762989, 4.238866729160403857, 11.69739621335923729 ) ) ;
#7519 = CARTESIAN_POINT ( 'NONE',  ( 16.56679352167444819, 0.008311568981097328460, -0.004162264567719685220 ) ) ;
#7520 = CARTESIAN_POINT ( 'NONE',  ( -66.35602477868049220, 9.999999999999973355, 11.00000000000000000 ) ) ;
#7521 = CARTESIAN_POINT ( 'NONE',  ( 1.846138399168762101, -11.69739621335919111, -4.238866729160527314 ) ) ;
#7522 = CARTESIAN_POINT ( 'NONE',  ( 16.56753206892534891, 0.008432171035096382855, 0.004368917149004273269 ) ) ;
#7523 = ORIENTED_EDGE ( 'NONE', *, *, #1778, .T. ) ;
#7524 = EDGE_LOOP ( 'NONE', ( #12727, #17677, #1738, #18276 ) ) ;
#7525 = ORIENTED_EDGE ( 'NONE', *, *, #17215, .T. ) ;
#7526 = VECTOR ( 'NONE', #5860, 1000.000000000000114 ) ;
#7527 = VERTEX_POINT ( 'NONE', #6792 ) ;
#7528 = EDGE_CURVE ( 'NONE', #2529, #1103, #957, .T. ) ;
#7529 = DIRECTION ( 'NONE',  ( 0.000000000000000000, 0.000000000000000000, 1.000000000000000000 ) ) ;
#7530 = EDGE_CURVE ( 'NONE', #14742, #10307, #12175, .T. ) ;
#7531 = DIRECTION ( 'NONE',  ( 0.000000000000000000, 0.000000000000000000, -1.000000000000000000 ) ) ;
#7532 = CARTESIAN_POINT ( 'NONE',  ( 0.3720661004400037664, -12.89739157014188997, -4.951033743989776248 ) ) ;
#7533 = VERTEX_POINT ( 'NONE', #18620 ) ;
#7534 = DIRECTION ( 'NONE',  ( 0.7635533937278214944, -0.6071939193889578368, -0.2197766120036483140 ) ) ;
#7535 = LINE ( 'NONE', #1593, #441 ) ;
#7536 = B_SPLINE_CURVE_WITH_KNOTS ( 'NONE', 3,
 ( #5282, #13887, #804, #15145, #11038, #10948 ),
 .UNSPECIFIED., .F., .F.,
 ( 4, 2, 4 ),
 ( 0.000000000000000000, 0.001656992708822505175, 0.003313985417645010350 ),
 .UNSPECIFIED. ) ;
#7537 = CARTESIAN_POINT ( 'NONE',  ( 3.943463214271659518E-15, -16.60000000000000142, 22.91316734529526045 ) ) ;
#7538 = CARTESIAN_POINT ( 'NONE',  ( 3.074695600507531434, 11.23985886659412259, 10.75417554975680900 ) ) ;
#7539 = CARTESIAN_POINT ( 'NONE',  ( 3.377929128793395908, -3.070552481924963217, 13.64476897106782971 ) ) ;
#7540 = ADVANCED_FACE ( 'NONE', ( #11195 ), #12056, .T. ) ;
#7541 = DIRECTION ( 'NONE',  ( 0.000000000000000000, 0.000000000000000000, 1.000000000000000000 ) ) ;
#7542 = CARTESIAN_POINT ( 'NONE',  ( 2.636624412715137922, -6.973567714907947135, 14.46769361191283920 ) ) ;
#7543 = DIRECTION ( 'NONE',  ( 0.000000000000000000, 0.000000000000000000, 1.000000000000000000 ) ) ;
#7544 = COLOUR_RGB ( '', 0.31764706, 0.68627451, 0.89019608) ;
#7545 = DIRECTION ( 'NONE',  ( 0.000000000000000000, 0.000000000000000000, -1.000000000000000000 ) ) ;
#7546 = ORIENTED_EDGE ( 'NONE', *, *, #13094, .F. ) ;
#7547 = VERTEX_POINT ( 'NONE', #12605 ) ;
#7548 = ORIENTED_EDGE ( 'NONE', *, *, #10715, .F. ) ;
#7549 = CIRCLE ( 'NONE', #8444, 5.000000000000004441 ) ;
#7550 = ORIENTED_EDGE ( 'NONE', *, *, #17793, .F. ) ;
#7551 = CARTESIAN_POINT ( 'NONE',  ( 1.918921323896210840, 9.738309537478938793, 7.860085869556105109 ) ) ;
#7552 = AXIS2_PLACEMENT_3D ( 'NONE', #7107, #9593, #11323 ) ;
#7553 = AXIS2_PLACEMENT_3D ( 'NONE', #13949, #2551, #8401 ) ;
#7554 = ORIENTED_EDGE ( 'NONE', *, *, #11935, .T. ) ;
#7555 = CARTESIAN_POINT ( 'NONE',  ( 0.3939875929385635578, -11.57636969881029110, -7.545068896001335013 ) ) ;
#7556 = EDGE_CURVE ( 'NONE', #17875, #11285, #8104, .T. ) ;
#7557 = CARTESIAN_POINT ( 'NONE',  ( 1.846138399168762989, 11.95493567637850774, 3.446241763653039580 ) ) ;
#7558 = CARTESIAN_POINT ( 'NONE',  ( 1.499999999999998668, 6.799999999999999822, 5.000000000000000000 ) ) ;
#7559 = B_SPLINE_CURVE_WITH_KNOTS ( 'NONE', 3,
 ( #5446, #11292, #17108, #6990, #12804, #4110 ),
 .UNSPECIFIED., .F., .F.,
 ( 4, 2, 4 ),
 ( 4.276569467073304015E-17, 0.0002014099069817285948, 0.0004028198139634144178 ),
 .UNSPECIFIED. ) ;
#7560 = SPHERICAL_SURFACE ( 'NONE', #3819, 5.315148208181397216 ) ;
#7561 = ORIENTED_EDGE ( 'NONE', *, *, #11967, .F. ) ;
#7562 = CARTESIAN_POINT ( 'NONE',  ( -1.876079424475003199, 7.500000000000000000, -15.16033210860608804 ) ) ;
#7563 = AXIS2_PLACEMENT_3D ( 'NONE', #17340, #18488, #8640 ) ;
#7564 = CARTESIAN_POINT ( 'NONE',  ( 0.3151930723728440520, 13.04315954105015152, 4.318364831037635021 ) ) ;
#7565 = B_SPLINE_CURVE_WITH_KNOTS ( 'NONE', 3,
 ( #11410, #12740, #8268, #9961, #13991, #5385, #18295, #5292, #16955, #4044, #11320, #12553, #4142 ),
 .UNSPECIFIED., .F., .F.,
 ( 4, 3, 3, 3, 4 ),
 ( 2.168404344971008868E-18, 0.0002299780670421057124, 0.0004599561239687910961, 0.0006896788984287892561, 0.0009194956271626406052 ),
 .UNSPECIFIED. ) ;
#7566 = CARTESIAN_POINT ( 'NONE',  ( -6.439472576468937781, 7.500000000000000000, -12.20506288372541093 ) ) ;
#7567 = CARTESIAN_POINT ( 'NONE',  ( 1.342453679581834924, 7.902645620902629453, -12.51077660954457293 ) ) ;
#7568 = CARTESIAN_POINT ( 'NONE',  ( 16.57778382496167424, 0.001819584982831895037, 0.01482878558584693578 ) ) ;
#7569 = CARTESIAN_POINT ( 'NONE',  ( 2.002547531651519996, -12.57989064830759141, -0.6781519942173057647 ) ) ;
#7570 = CIRCLE ( 'NONE', #1438, 14.54644660717763927 ) ;
#7571 =( REPRESENTATION_RELATIONSHIP ('NONE','NONE', #5200, #16816 ) REPRESENTATION_RELATIONSHIP_WITH_TRANSFORMATION ( #1173 )SHAPE_REPRESENTATION_RELATIONSHIP( ) );
#7572 = AXIS2_PLACEMENT_3D ( 'NONE', #15697, #8443, #11413 ) ;
#7573 = EDGE_CURVE ( 'NONE', #1448, #9140, #14796, .T. ) ;
#7574 = CARTESIAN_POINT ( 'NONE',  ( 16.56679352167444819, 0.004277682826583292797, 0.008252760440870202802 ) ) ;
#7575 = ORIENTED_EDGE ( 'NONE', *, *, #16940, .T. ) ;
#7576 = CARTESIAN_POINT ( 'NONE',  ( 1.977436885025838142, -14.12046670317529440, -6.153171729168441573 ) ) ;
#7578 = ORIENTED_EDGE ( 'NONE', *, *, #11083, .T. ) ;
#7577 = CARTESIAN_POINT ( 'NONE',  ( 2.002547531651520885, 10.57595306287292480, 6.845637710436228929 ) ) ;
#7579 = CARTESIAN_POINT ( 'NONE',  ( 1.846138399168762101, -11.69739621335919111, -4.238866729160527314 ) ) ;
#7580 = LINE ( 'NONE', #17891, #379 ) ;
#7581 = B_SPLINE_CURVE_WITH_KNOTS ( 'NONE', 3,
 ( #2953, #8801, #14624, #2119, #3635, #7671 ),
 .UNSPECIFIED., .F., .F.,
 ( 4, 2, 4 ),
 ( 3.522439207679730663E-17, 0.0001825746017570583171, 0.0003651492035140813976 ),
 .UNSPECIFIED. ) ;
#7582 = VECTOR ( 'NONE', #465, 1000.000000000000000 ) ;
#7583 = ORIENTED_EDGE ( 'NONE', *, *, #11417, .F. ) ;
#7584 = FACE_OUTER_BOUND ( 'NONE', #16017, .T. ) ;
#7585 = CARTESIAN_POINT ( 'NONE',  ( 5.704021078595903127, -7.499999999999735323, -12.80826310103411991 ) ) ;
#7586 = ORIENTED_EDGE ( 'NONE', *, *, #6910, .T. ) ;
#7587 = CARTESIAN_POINT ( 'NONE',  ( 16.56872352241294521, -0.01033355228142402750, 0.001442253899401767583 ) ) ;
#7588 = CARTESIAN_POINT ( 'NONE',  ( 0.4862570985993235340, -10.79774104611366781, -8.769551628660854803 ) ) ;
#7589 = CARTESIAN_POINT ( 'NONE',  ( 0.3307726912345213544, -10.76786801061213161, 8.558645027434234720 ) ) ;
#7590 = DIRECTION ( 'NONE',  ( 0.000000000000000000, 0.000000000000000000, 1.000000000000000000 ) ) ;
#7591 = EDGE_CURVE ( 'NONE', #7599, #14770, #1674, .T. ) ;
#7592 = AXIS2_PLACEMENT_3D ( 'NONE', #6147, #5152, #17810 ) ;
#7593 = FILL_AREA_STYLE_COLOUR ( '', #10906 ) ;
#7594 = CARTESIAN_POINT ( 'NONE',  ( 5.000000000000000000, 6.123233995736766282E-16, 0.000000000000000000 ) ) ;
#7595 = DIRECTION ( 'NONE',  ( -0.000000000000000000, -1.000000000000000000, -0.000000000000000000 ) ) ;
#7596 = CARTESIAN_POINT ( 'NONE',  ( 16.56822296793089322, -0.006547366384935564970, 0.007741272030791060237 ) ) ;
#7597 = CARTESIAN_POINT ( 'NONE',  ( 0.3137051932979792457, 11.37800749014131263, 7.698472063774513430 ) ) ;
#7598 = FACE_OUTER_BOUND ( 'NONE', #8758, .T. ) ;
#7599 = VERTEX_POINT ( 'NONE', #13955 ) ;
#7600 = CARTESIAN_POINT ( 'NONE',  ( 16.57778382496167424, 0.01092721432668994352, 0.01018821665058780926 ) ) ;
#7601 = DIRECTION ( 'NONE',  ( 0.000000000000000000, 0.000000000000000000, 1.000000000000000000 ) ) ;
#7602 = AXIS2_PLACEMENT_3D ( 'NONE', #12728, #16757, #18555 ) ;
#7603 = ORIENTED_EDGE ( 'NONE', *, *, #3410, .T. ) ;
#7604 = ORIENTED_EDGE ( 'NONE', *, *, #434, .T. ) ;
#7605 = DIRECTION ( 'NONE',  ( -1.000000000000000000, 0.000000000000000000, 0.000000000000000000 ) ) ;
#7606 = ORIENTED_EDGE ( 'NONE', *, *, #7390, .F. ) ;
#7607 = CARTESIAN_POINT ( 'NONE',  ( -66.35602477868047799, -10.00000000000000888, 3.000000000000000000 ) ) ;
#7608 = ORIENTED_EDGE ( 'NONE', *, *, #16394, .T. ) ;
#7609 = CARTESIAN_POINT ( 'NONE',  ( 1.321128355694181398E-14, -7.013167318348350499, 25.01316734529530095 ) ) ;
#7610 = CARTESIAN_POINT ( 'NONE',  ( 0.3095370825347224519, -0.4597470195091133416, 13.73357284481724605 ) ) ;
#7611 = CARTESIAN_POINT ( 'NONE',  ( 8.522092701127531811, -5.397361180353110299, -4.388629235579637466 ) ) ;
#7612 = B_SPLINE_CURVE_WITH_KNOTS ( 'NONE', 3,
 ( #18839, #5827, #7001, #11672 ),
 .UNSPECIFIED., .F., .F.,
 ( 4, 4 ),
 ( 0.000000000000000000, 0.002004993803842712932 ),
 .UNSPECIFIED. ) ;
#7613 = FACE_OUTER_BOUND ( 'NONE', #15130, .T. ) ;
#7614 = LINE ( 'NONE', #2065, #6282 ) ;
#7615 = B_SPLINE_CURVE_WITH_KNOTS ( 'NONE', 3,
 ( #10863, #16686, #3388, #3587, #545, #15245 ),
 .UNSPECIFIED., .F., .F.,
 ( 4, 2, 4 ),
 ( 1.084202172485504434E-19, 0.0002017457492448070664, 0.0004034914984896140243 ),
 .UNSPECIFIED. ) ;
#7616 = FILL_AREA_STYLE ('',( #13327 ) ) ;
#7617 = CARTESIAN_POINT ( 'NONE',  ( 0.4754618798421167414, -8.775436892861188554, 10.80499583390510132 ) ) ;
#7618 = ADVANCED_FACE ( 'NONE', ( #16241 ), #10506, .F. ) ;
#7619 = DIRECTION ( 'NONE',  ( -1.000000000000000000, 0.000000000000000000, 0.000000000000000000 ) ) ;
#7620 = CARTESIAN_POINT ( 'NONE',  ( 16.56872352241294521, 0.004907101719994633009, -0.009207754980063766539 ) ) ;
#7621 = DIRECTION ( 'NONE',  ( 0.000000000000000000, 1.000000000000000000, 0.000000000000000000 ) ) ;
#7622 = CARTESIAN_POINT ( 'NONE',  ( 1.846955891736117072, -11.74973605926567188, 4.094751675596655538 ) ) ;
#7623 = CARTESIAN_POINT ( 'NONE',  ( 0.3720661004400037664, 11.58636699658225844, -7.524064345033335321 ) ) ;
#7624 = VECTOR ( 'NONE', #2588, 1000.000000000000000 ) ;
#7625 = VERTEX_POINT ( 'NONE', #4584 ) ;
#7626 = EDGE_LOOP ( 'NONE', ( #8783, #8005, #10042, #12268 ) ) ;
#7627 = ORIENTED_EDGE ( 'NONE', *, *, #11637, .T. ) ;
#7628 = ORIENTED_EDGE ( 'NONE', *, *, #13219, .T. ) ;
#7629 = CIRCLE ( 'NONE', #3016, 4.000000000000000000 ) ;
#7630 = CARTESIAN_POINT ( 'NONE',  ( 0.3151928476913555821, -8.075884471919669849, -11.11514699826559571 ) ) ;
#7631 = DIRECTION ( 'NONE',  ( -0.7635533937278214944, 0.2197766120036462600, 0.6071939193889586139 ) ) ;
#7632 = DIRECTION ( 'NONE',  ( 0.000000000000000000, 0.000000000000000000, -1.000000000000000000 ) ) ;
#7633 = CARTESIAN_POINT ( 'NONE',  ( -1.979226605763932723, -19.99999999999999645, 6.000000000000000000 ) ) ;
#7634 = DIRECTION ( 'NONE',  ( 0.000000000000000000, 0.000000000000000000, 1.000000000000000000 ) ) ;
#7635 = AXIS2_PLACEMENT_3D ( 'NONE', #2293, #3918, #12702 ) ;
#7636 = CARTESIAN_POINT ( 'NONE',  ( 0.3058872367615226295, 0.6080468242582872662, -13.72992299905059177 ) ) ;
#7637 = CARTESIAN_POINT ( 'NONE',  ( -61.35602477868047799, -10.00000000000000888, 3.000000000000000000 ) ) ;
#7638 = CARTESIAN_POINT ( 'NONE',  ( 1.847247051441591514, 12.44188156437794390, 0.1676840720645733362 ) ) ;
#7639 = EDGE_CURVE ( 'NONE', #6997, #13145, #1665, .T. ) ;
#7640 = ADVANCED_FACE ( 'NONE', ( #14512 ), #14699, .F. ) ;
#7641 = FACE_OUTER_BOUND ( 'NONE', #3291, .T. ) ;
#7642 = CARTESIAN_POINT ( 'NONE',  ( 16.56822296793089322, 0.002414375228568836022, 0.009847136207495320662 ) ) ;
#7643 = EDGE_CURVE ( 'NONE', #16490, #4199, #13760, .T. ) ;
#7644 = DIRECTION ( 'NONE',  ( -0.000000000000000000, 0.000000000000000000, 1.000000000000000000 ) ) ;
#7645 =( BOUNDED_SURFACE ( )  B_SPLINE_SURFACE ( 3, 1, ( 
 ( #12621, #5365 ),
 ( #16934, #1247 ),
 ( #12445, #11301 ),
 ( #14256, #18277 ) ),
 .UNSPECIFIED., .F., .F., .T. ) 
 B_SPLINE_SURFACE_WITH_KNOTS ( ( 4, 4 ),
 ( 2, 2 ),
 ( 0.000000000000000000, 1.000000000000000000 ),
 ( 0.000000000000000000, 1.000000000000000000 ),
 .UNSPECIFIED. ) 
 GEOMETRIC_REPRESENTATION_ITEM ( )  RATIONAL_B_SPLINE_SURFACE ( (
 ( 1.000000000000000000, 1.000000000000000000),
 ( 0.7792777138730158093, 0.9689936506012928330),
 ( 0.7792777138730158093, 0.9689936506012928330),
 ( 1.000000000000000000, 1.000000000000000000) ) ) 
 REPRESENTATION_ITEM ( '' )  SURFACE ( )  );
#7646 = CARTESIAN_POINT ( 'NONE',  ( 12.00000000000000711, -14.99999999999999645, 8.000000000000000000 ) ) ;
#7647 = ORIENTED_EDGE ( 'NONE', *, *, #14005, .T. ) ;
#7648 = ORIENTED_EDGE ( 'NONE', *, *, #7117, .T. ) ;
#7649 = EDGE_LOOP ( 'NONE', ( #6563, #639, #17574, #12901 ) ) ;
#7650 = B_SPLINE_CURVE_WITH_KNOTS ( 'NONE', 3,
 ( #10717, #16820, #5154, #6417, #15006, #3722 ),
 .UNSPECIFIED., .F., .F.,
 ( 4, 2, 4 ),
 ( 4.878909776184769953E-19, 0.001657017934711441055, 0.003314035869422881676 ),
 .UNSPECIFIED. ) ;
#7651 = EDGE_LOOP ( 'NONE', ( #7116, #14089, #8920, #6676 ) ) ;
#7652 = DIRECTION ( 'NONE',  ( 0.000000000000000000, 0.000000000000000000, 1.000000000000000000 ) ) ;
#7653 = CARTESIAN_POINT ( 'NONE',  ( 16.56872352241294521, 0.001442253899401220278, -0.01033355228142500415 ) ) ;
#7654 = CARTESIAN_POINT ( 'NONE',  ( -30.00000000000000355, -12.50000000000000178, -1.000000000000000000 ) ) ;
#7655 = CARTESIAN_POINT ( 'NONE',  ( 2.697797270744671128, 10.19107313879056953, 8.537712152180894520 ) ) ;
#7656 = CARTESIAN_POINT ( 'NONE',  ( 20.00000000000000711, -39.99999999999999289, 3.000000000000000000 ) ) ;
#7657 = ORIENTED_EDGE ( 'NONE', *, *, #14202, .F. ) ;
#7658 = CARTESIAN_POINT ( 'NONE',  ( 0.5553368343811782015, 7.500000000000000000, -14.29382045140261503 ) ) ;
#7659 = DIRECTION ( 'NONE',  ( 0.000000000000000000, 0.000000000000000000, -1.000000000000000000 ) ) ;
#7660 = CARTESIAN_POINT ( 'NONE',  ( -20.00000000000000000, -2.500000000000000444, -16.99999999999999645 ) ) ;
#7661 = CARTESIAN_POINT ( 'NONE',  ( 0.3137051932979775248, -0.4596302728638797519, -13.73004976592202553 ) ) ;
#7662 = DIRECTION ( 'NONE',  ( 1.000000000000000000, 0.000000000000000000, 0.000000000000000000 ) ) ;
#7663 = FILL_AREA_STYLE ('',( #14907 ) ) ;
#7664 = AXIS2_PLACEMENT_3D ( 'NONE', #12821, #5549, #11399 ) ;
#7665 = CARTESIAN_POINT ( 'NONE',  ( 2.179449471770337432, -4.500000000000000000, -6.000000000000000000 ) ) ;
#7666 = VERTEX_POINT ( 'NONE', #7458 ) ;
#7667 = ADVANCED_FACE ( 'NONE', ( #16343 ), #3124, .T. ) ;
#7668 = DIRECTION ( 'NONE',  ( -1.540743955509788340E-33, -1.000000000000000000, -2.533398541561209262E-17 ) ) ;
#7670 = VERTEX_POINT ( 'NONE', #5707 ) ;
#7669 = DIRECTION ( 'NONE',  ( 0.7635533937278216055, 0.6071939193889560604, 0.2197766120036526161 ) ) ;
#7671 = CARTESIAN_POINT ( 'NONE',  ( 1.846138399168762989, 11.95493567637850774, 3.446241763653039580 ) ) ;
#7672 = CARTESIAN_POINT ( 'NONE',  ( 8.438534575730034959, -5.415535776177550886, 4.221456476902647914 ) ) ;
#7673 = ORIENTED_EDGE ( 'NONE', *, *, #16056, .T. ) ;
#7674 = CARTESIAN_POINT ( 'NONE',  ( 3.512766787570801519, 6.535475144496956545, 13.55823433651946175 ) ) ;
#7675 = CARTESIAN_POINT ( 'NONE',  ( 1.149093537842186707, -7.500000000000000888, -14.62468756229394629 ) ) ;
#7676 =( BOUNDED_SURFACE ( )  B_SPLINE_SURFACE ( 3, 1, ( 
 ( #7852, #6594 ),
 ( #15098, #16631 ),
 ( #13672, #2372 ),
 ( #16728, #12420 ) ),
 .UNSPECIFIED., .F., .F., .T. ) 
 B_SPLINE_SURFACE_WITH_KNOTS ( ( 4, 4 ),
 ( 2, 2 ),
 ( 0.000000000000000000, 1.000000000000000000 ),
 ( 0.000000000000000000, 1.000000000000000000 ),
 .UNSPECIFIED. ) 
 GEOMETRIC_REPRESENTATION_ITEM ( )  RATIONAL_B_SPLINE_SURFACE ( (
 ( 1.000000000000000000, 1.000000000000000000),
 ( 0.9933953342250438912, 0.8357391271907739227),
 ( 0.9933953342250438912, 0.8357391271907739227),
 ( 1.000000000000000000, 1.000000000000000000) ) ) 
 REPRESENTATION_ITEM ( '' )  SURFACE ( )  );
#7677 = EDGE_LOOP ( 'NONE', ( #3193, #7384, #18364, #9362 ) ) ;
#7678 = CARTESIAN_POINT ( 'NONE',  ( 8.522092701127531811, -5.841710761610158009, 3.777034505568503064 ) ) ;
#7679 = CARTESIAN_POINT ( 'NONE',  ( 1.560000000000000053, 0.000000000000000000, 0.000000000000000000 ) ) ;
#7680 = APPLICATION_CONTEXT ( 'automotive_design' ) ;
#7681 = FACE_OUTER_BOUND ( 'NONE', #15058, .T. ) ;
#7682 = DIRECTION ( 'NONE',  ( -1.000000000000000000, -0.000000000000000000, -0.000000000000000000 ) ) ;
#7683 = VECTOR ( 'NONE', #10102, 1000.000000000000000 ) ;
#7684 = EDGE_LOOP ( 'NONE', ( #1956, #8939, #775, #2181 ) ) ;
#7685 = EDGE_CURVE ( 'NONE', #11625, #15676, #3026, .T. ) ;
#7686 = CARTESIAN_POINT ( 'NONE',  ( 2.002547531651519996, 12.17374746633578475, 3.242439124566693476 ) ) ;
#7687 = CARTESIAN_POINT ( 'NONE',  ( 0.3151926232592466848, 11.16039997398654116, 8.013596737356428079 ) ) ;
#7688 = EDGE_CURVE ( 'NONE', #1566, #16455, #13884, .T. ) ;
#7689 = DIRECTION ( 'NONE',  ( -1.000000000000000000, -0.000000000000000000, -0.000000000000000000 ) ) ;
#7691 = ORIENTED_EDGE ( 'NONE', *, *, #18650, .F. ) ;
#7690 = FACE_OUTER_BOUND ( 'NONE', #9446, .T. ) ;
#7692 = CARTESIAN_POINT ( 'NONE',  ( 0.4862570985993235340, -13.89016912371016943, -0.7479633556563904939 ) ) ;
#7693 = ORIENTED_EDGE ( 'NONE', *, *, #7516, .F. ) ;
#7694 = CARTESIAN_POINT ( 'NONE',  ( 0.3145734862173260038, -4.535879238195024143, 12.96846406299304988 ) ) ;
#7695 = CARTESIAN_POINT ( 'NONE',  ( -66.35602477868047799, 9.999999999999973355, 3.000000000000000000 ) ) ;
#7696 = ORIENTED_EDGE ( 'NONE', *, *, #5290, .F. ) ;
#7697 = VERTEX_POINT ( 'NONE', #11941 ) ;
#7699 = CARTESIAN_POINT ( 'NONE',  ( 1.846524061778019199, -0.3544704288993353880, 12.43723828841088341 ) ) ;
#7698 = AXIS2_PLACEMENT_3D ( 'NONE', #14253, #9752, #9666 ) ;
#7700 = EDGE_LOOP ( 'NONE', ( #15549, #5162, #3099, #5314 ) ) ;
#7701 = DIRECTION ( 'NONE',  ( -1.000000000000000000, 0.000000000000000000, -0.000000000000000000 ) ) ;
#7702 = ORIENTED_EDGE ( 'NONE', *, *, #17661, .T. ) ;
#7703 = EDGE_CURVE ( 'NONE', #12288, #17352, #956, .T. ) ;
#7704 = SURFACE_STYLE_USAGE ( .BOTH. , #6450 ) ;
#7705 = DIRECTION ( 'NONE',  ( 0.000000000000000000, 0.000000000000000000, 1.000000000000000000 ) ) ;
#7706 = FACE_OUTER_BOUND ( 'NONE', #58, .T. ) ;
#7707 = CARTESIAN_POINT ( 'NONE',  ( 0.3151930723728439410, 4.172946285306569969, 13.09040889075571990 ) ) ;
#7708 = PRODUCT ( 'Soft-Grip Handle Sleeve Overmolds (x2)', 'Soft-Grip Handle Sleeve Overmolds (x2)', '', ( #5109 ) ) ;
#7709 = CARTESIAN_POINT ( 'NONE',  ( 3.950837973638668288, 0.000000000000000000, 0.000000000000000000 ) ) ;
#7710 = CARTESIAN_POINT ( 'NONE',  ( 16.58200780006414732, 0.01080144354108992025, -0.002844973367390922145 ) ) ;
#7711 = SHAPE_REPRESENTATION_RELATIONSHIP ( 'NONE' , 'NONE' ,  #8995, #2583 ) ;
#7712 = FACE_OUTER_BOUND ( 'NONE', #9976, .T. ) ;
#7713 = CARTESIAN_POINT ( 'NONE',  ( 2.320520222539219635, -3.126729907238178896, -15.43440824796753930 ) ) ;
#7714 = CARTESIAN_POINT ( 'NONE',  ( 0.3142014840576498047, 7.762239086932858356, 11.33546131209465102 ) ) ;
#7715 = CARTESIAN_POINT ( 'NONE',  ( 2.002547531651519996, 11.75462648437101976, 4.532360870844369671 ) ) ;
#7716 = CARTESIAN_POINT ( 'NONE',  ( 1.847247051441591514, -11.88474976472815214, 3.685275815977142599 ) ) ;
#7717 = CARTESIAN_POINT ( 'NONE',  ( 0.3137051932979792457, 0.4596302728641686874, -13.73004976592201487 ) ) ;
#7718 = VERTEX_POINT ( 'NONE', #10214 ) ;
#7719 = EDGE_CURVE ( 'NONE', #14456, #13838, #14605, .T. ) ;
#7720 = EDGE_LOOP ( 'NONE', ( #13264, #11664, #14159, #15234 ) ) ;
#7721 = ORIENTED_EDGE ( 'NONE', *, *, #15101, .T. ) ;
#7722 = VERTEX_POINT ( 'NONE', #13173 ) ;
#7723 = ADVANCED_FACE ( 'NONE', ( #89 ), #5386, .F. ) ;
#7724 = CARTESIAN_POINT ( 'NONE',  ( 0.3137051932979809665, 10.83767969834803324, 8.442169467526891680 ) ) ;
#7725 = CARTESIAN_POINT ( 'NONE',  ( 1.846138399168762101, -12.43476674860266940, 0.4167076046095114505 ) ) ;
#7726 = SPHERICAL_SURFACE ( 'NONE', #10204, 5.000000000000000000 ) ;
#7727 = CARTESIAN_POINT ( 'NONE',  ( 3.512766787570769544, 10.87507422923904166, -10.40533104696121214 ) ) ;
#7728 = PRODUCT_DEFINITION_CONTEXT ( 'detailed design', #17804, 'design' ) ;
#7729 = CARTESIAN_POINT ( 'NONE',  ( 0.000000000000000000, 0.000000000000000000, 0.000000000000000000 ) ) ;
#7730 = CARTESIAN_POINT ( 'NONE',  ( 3.950837973638668288, 0.000000000000000000, 0.000000000000000000 ) ) ;
#7731 = CARTESIAN_POINT ( 'NONE',  ( 0.3145729642390364678, 8.321438378985256179, 10.93201268464375353 ) ) ;
#7732 = CYLINDRICAL_SURFACE ( 'NONE', #15424, 4.750000000000000000 ) ;
#7733 = CARTESIAN_POINT ( 'NONE',  ( 2.320521194581858460, 15.43440938316986610, 3.126729093672275805 ) ) ;
#7734 = CARTESIAN_POINT ( 'NONE',  ( 0.3095370825347224519, 0.4597470195090193057, 13.73357284481724960 ) ) ;
#7735 = DIRECTION ( 'NONE',  ( 7.059849041517224761E-27, 1.000000000000000000, -1.472402716619196496E-26 ) ) ;
#7736 = CARTESIAN_POINT ( 'NONE',  ( 1.847247051441591292, 7.177495230324704600, 10.16425585218603267 ) ) ;
#7737 = AXIS2_PLACEMENT_3D ( 'NONE', #3182, #2990, #6168 ) ;
#7738 = EDGE_LOOP ( 'NONE', ( #327, #12577, #3137, #9674, #18841 ) ) ;
#7739 = ORIENTED_EDGE ( 'NONE', *, *, #16194, .T. ) ;
#7740 = ORIENTED_EDGE ( 'NONE', *, *, #1312, .T. ) ;
#7741 = VERTEX_POINT ( 'NONE', #14898 ) ;
#7742 = DIRECTION ( 'NONE',  ( 0.000000000000000000, 1.224646799147353207E-16, -1.000000000000000000 ) ) ;
#7743 = EDGE_CURVE ( 'NONE', #3320, #10843, #1629, .T. ) ;
#7744 = EDGE_CURVE ( 'NONE', #10843, #4344, #16230, .T. ) ;
#7745 = EDGE_CURVE ( 'NONE', #15231, #16174, #10702, .T. ) ;
#7746 = CARTESIAN_POINT ( 'NONE',  ( 1.560000000000000053, -0.8660254037844384856, 1.500000000000000000 ) ) ;
#7747 = CARTESIAN_POINT ( 'NONE',  ( 5.000000000000000000, 6.123233995736766282E-16, 3.000000000000000000 ) ) ;
#7748 = FACE_BOUND ( 'NONE', #1882, .T. ) ;
#7749 = CARTESIAN_POINT ( 'NONE',  ( 4.755015822784811164, -4.336808689942017736E-16, 0.000000000000000000 ) ) ;
#7750 = ORIENTED_EDGE ( 'NONE', *, *, #14203, .F. ) ;
#7751 = CARTESIAN_POINT ( 'NONE',  ( 2.066926351139553475, 7.499999999999999112, -15.30321684074790056 ) ) ;
#7752 = CONICAL_SURFACE ( 'NONE', #18696, 12.50000000000000355, 1.308996938995747428 ) ;
#7753 = CARTESIAN_POINT ( 'NONE',  ( 16.56872352241294521, 0.009382111268607367521, 0.004564908236399998868 ) ) ;
#7754 = CARTESIAN_POINT ( 'NONE',  ( 1.342453679581834924, -7.902645620902536194, 12.51077660954462978 ) ) ;
#7755 = CARTESIAN_POINT ( 'NONE',  ( 1.847034903785822468, -10.19974412751570014, 7.126331315909236075 ) ) ;
#7756 =( BOUNDED_SURFACE ( )  B_SPLINE_SURFACE ( 3, 1, ( 
 ( #18111, #5013 ),
 ( #15242, #16683 ),
 ( #2156, #2499 ),
 ( #6918, #987 ) ),
 .UNSPECIFIED., .F., .F., .T. ) 
 B_SPLINE_SURFACE_WITH_KNOTS ( ( 4, 4 ),
 ( 2, 2 ),
 ( 0.000000000000000000, 1.000000000000000000 ),
 ( 0.000000000000000000, 1.000000000000000000 ),
 .UNSPECIFIED. ) 
 GEOMETRIC_REPRESENTATION_ITEM ( )  RATIONAL_B_SPLINE_SURFACE ( (
 ( 1.000000000000000000, 1.000000000000000000),
 ( 0.9933953342250438912, 0.8357391271907739227),
 ( 0.9933953342250438912, 0.8357391271907739227),
 ( 1.000000000000000000, 1.000000000000000000) ) ) 
 REPRESENTATION_ITEM ( '' )  SURFACE ( )  );
#7757 = FACE_OUTER_BOUND ( 'NONE', #14768, .T. ) ;
#7758 = CARTESIAN_POINT ( 'NONE',  ( 8.438534575730034959, 0.2320579683290127926, 6.862570336891076650 ) ) ;
#7759 = EDGE_CURVE ( 'NONE', #10243, #10742, #15089, .T. ) ;
#7760 = ORIENTED_EDGE ( 'NONE', *, *, #4517, .T. ) ;
#7761 = CARTESIAN_POINT ( 'NONE',  ( 2.320521194582656044, -11.60169518685945356, 10.64885423995117542 ) ) ;
#7763 = ORIENTED_EDGE ( 'NONE', *, *, #1125, .F. ) ;
#7762 = CARTESIAN_POINT ( 'NONE',  ( 1.562796894703937678, 0.000000000000000000, 2.500000000000000000 ) ) ;
#7764 = CARTESIAN_POINT ( 'NONE',  ( 3.950837973638676281, -14.41405733518061716, 1.958075594453740687 ) ) ;
#7765 = CARTESIAN_POINT ( 'NONE',  ( 0.3939875929385612263, 10.75308190953755982, -8.678227324501007089 ) ) ;
#7766 = VERTEX_POINT ( 'NONE', #3524 ) ;
#7767 = CARTESIAN_POINT ( 'NONE',  ( -66.35602477868047799, -10.00000000000000888, 3.000000000000002665 ) ) ;
#7768 = CARTESIAN_POINT ( 'NONE',  ( -0.2197594725757872069, -7.499999999999768185, -13.03330426733007386 ) ) ;
#7769 = ORIENTED_EDGE ( 'NONE', *, *, #18587, .F. ) ;
#7770 = CARTESIAN_POINT ( 'NONE',  ( 2.123976203522053741, 7.899625852120402136, -13.47898556379304580 ) ) ;
#7771 = CARTESIAN_POINT ( 'NONE',  ( 16.56872352241294521, -0.007240717549633941472, -0.007512283835804289302 ) ) ;
#7772 = EDGE_CURVE ( 'NONE', #9529, #10646, #15703, .T. ) ;
#7773 = CARTESIAN_POINT ( 'NONE',  ( 0.4384471787762838635, -10.76632603192792459, 8.732395932355645485 ) ) ;
#7774 = CARTESIAN_POINT ( 'NONE',  ( 1.847372867223022519, 10.12831093686732586, -7.228345833872643844 ) ) ;
#7775 = CONICAL_SURFACE ( 'NONE', #17509, 14.54644660717763927, 0.8559913436420816257 ) ;
#7776 = AXIS2_PLACEMENT_3D ( 'NONE', #17268, #17176, #18607 ) ;
#7777 = ORIENTED_EDGE ( 'NONE', *, *, #17094, .F. ) ;
#7778 = ORIENTED_EDGE ( 'NONE', *, *, #3886, .F. ) ;
#7779 = EDGE_CURVE ( 'NONE', #13879, #11517, #6586, .T. ) ;
#7780 = CARTESIAN_POINT ( 'NONE',  ( 2.636624412715138366, -15.91454522070249311, -2.161493821597819665 ) ) ;
#7781 = CARTESIAN_POINT ( 'NONE',  ( -11.50000000000000178, 1.408343819019456373E-15, 10.49999999999999822 ) ) ;
#7783 = VERTEX_POINT ( 'NONE', #577 ) ;
#7782 = CARTESIAN_POINT ( 'NONE',  ( 1.846138399168762101, 10.30487220521580305, -6.971848976710897539 ) ) ;
#7784 = FACE_OUTER_BOUND ( 'NONE', #13289, .T. ) ;
#7785 = EDGE_LOOP ( 'NONE', ( #11308, #2625 ) ) ;
#7786 = CARTESIAN_POINT ( 'NONE',  ( 16.56872352241294521, 0.01033355228142401709, -0.001442253899401843694 ) ) ;
#7787 =( BOUNDED_SURFACE ( )  B_SPLINE_SURFACE ( 3, 1, ( 
 ( #7245, #9804 ),
 ( #15634, #2536 ),
 ( #14217, #1113 ),
 ( #6965, #12776 ) ),
 .UNSPECIFIED., .F., .F., .T. ) 
 B_SPLINE_SURFACE_WITH_KNOTS ( ( 4, 4 ),
 ( 2, 2 ),
 ( 0.000000000000000000, 1.000000000000000000 ),
 ( 0.000000000000000000, 1.000000000000000000 ),
 .UNSPECIFIED. ) 
 GEOMETRIC_REPRESENTATION_ITEM ( )  RATIONAL_B_SPLINE_SURFACE ( (
 ( 1.000000000000000000, 1.000000000000000000),
 ( 0.9933953342250436691, 0.8357391271907733676),
 ( 0.9933953342250436691, 0.8357391271907733676),
 ( 1.000000000000000000, 1.000000000000000000) ) ) 
 REPRESENTATION_ITEM ( '' )  SURFACE ( )  );
#7788 = CARTESIAN_POINT ( 'NONE',  ( 2.320520222537495680, -11.60169517779343096, -10.64885284335084847 ) ) ;
#7789 = ORIENTED_EDGE ( 'NONE', *, *, #15765, .T. ) ;
#7790 = VECTOR ( 'NONE', #8007, 1000.000000000000000 ) ;
#7791 = ORIENTED_EDGE ( 'NONE', *, *, #17124, .T. ) ;
#7792 = CARTESIAN_POINT ( 'NONE',  ( -30.00000000000000355, -12.50000000000000178, -0.5000000000000000000 ) ) ;
#7793 = ORIENTED_EDGE ( 'NONE', *, *, #18312, .T. ) ;
#7794 = PLANE ( 'NONE',  #11745 ) ;
#7795 = ORIENTED_EDGE ( 'NONE', *, *, #17118, .F. ) ;
#7796 = CIRCLE ( 'NONE', #9597, 5.000000000000000000 ) ;
#7797 =( LENGTH_UNIT ( ) NAMED_UNIT ( * ) SI_UNIT ( .MILLI., .METRE. ) );
#7798 = CIRCLE ( 'NONE', #17545, 16.06066017081991149 ) ;
#7799 = DIRECTION ( 'NONE',  ( 0.000000000000000000, 0.000000000000000000, -1.000000000000000000 ) ) ;
#7800 = B_SPLINE_CURVE_WITH_KNOTS ( 'NONE', 3,
 ( #11013, #11105, #9562, #6796, #15119, #15393 ),
 .UNSPECIFIED., .F., .F.,
 ( 4, 2, 4 ),
 ( 1.946286347258496500E-18, 0.0002017457492448080964, 0.0004034914984896142412 ),
 .UNSPECIFIED. ) ;
#7801 = CARTESIAN_POINT ( 'NONE',  ( 0.4384471787762834749, 13.84291427302851574, -0.7363690479466810102 ) ) ;
#7802 = CARTESIAN_POINT ( 'NONE',  ( 0.3137051932979757485, -7.698472063774552510, 11.37800749014128421 ) ) ;
#7803 = B_SPLINE_CURVE_WITH_KNOTS ( 'NONE', 3,
 ( #16304, #17446, #11807, #5769, #2799, #7518 ),
 .UNSPECIFIED., .F., .F.,
 ( 4, 2, 4 ),
 ( 3.332294980281255979E-17, 0.0001825746017570583984, 0.0003651492035140835118 ),
 .UNSPECIFIED. ) ;
#7804 = DIRECTION ( 'NONE',  ( 0.000000000000000000, 0.000000000000000000, -1.000000000000000000 ) ) ;
#7805 = DIRECTION ( 'NONE',  ( 1.000000000000000000, 0.000000000000000000, 0.000000000000000000 ) ) ;
#7806 = EDGE_CURVE ( 'NONE', #16885, #570, #3423, .T. ) ;
#7807 = CARTESIAN_POINT ( 'NONE',  ( 0.4862570985993235340, 0.7479633556564388996, -13.89016912371016765 ) ) ;
#7808 = VECTOR ( 'NONE', #1939, 1000.000000000000000 ) ;
#7809 = CIRCLE ( 'NONE', #18459, 5.000000000000004441 ) ;
#7810 = CARTESIAN_POINT ( 'NONE',  ( 1.847372867223025183, 7.398914411685134418, -10.00438561114516034 ) ) ;
#7811 = VECTOR ( 'NONE', #4773, 1000.000000000000227 ) ;
#7812 = LINE ( 'NONE', #16774, #9376 ) ;
#7813 = EDGE_CURVE ( 'NONE', #18612, #16214, #7119, .T. ) ;
#7814 = DIRECTION ( 'NONE',  ( -1.000000000000000000, -0.000000000000000000, -0.000000000000000000 ) ) ;
#7815 = LINE ( 'NONE', #5116, #5099 ) ;
#7816 = VERTEX_POINT ( 'NONE', #377 ) ;
#7817 = VERTEX_POINT ( 'NONE', #16719 ) ;
#7818 = EDGE_LOOP ( 'NONE', ( #11740, #16870, #16374, #3940 ) ) ;
#7819 = ORIENTED_EDGE ( 'NONE', *, *, #7066, .F. ) ;
#7820 = CARTESIAN_POINT ( 'NONE',  ( 1.321128355694181398E-14, -8.013167318348349610, 37.51316734529530805 ) ) ;
#7821 = VECTOR ( 'NONE', #5864, 1000.000000000000114 ) ;
#7822 = DIRECTION ( 'NONE',  ( -0.000000000000000000, -0.5000000000000004441, 0.8660254037844383745 ) ) ;
#7823 = AXIS2_PLACEMENT_3D ( 'NONE', #11155, #2518, #7033 ) ;
#7824 = CARTESIAN_POINT ( 'NONE',  ( 1.847247051441592403, -12.44188156437794035, -0.1676840720646602112 ) ) ;
#7825 = CARTESIAN_POINT ( 'NONE',  ( 3.664313757352960721, 14.16986885736091750, 1.627055439596312159 ) ) ;
#7826 = CARTESIAN_POINT ( 'NONE',  ( 3.950837973638676281, -6.888253895133199300, -12.81214529934982949 ) ) ;
#7827 = DIRECTION ( 'NONE',  ( -1.000000000000000000, 0.000000000000000000, 0.000000000000000000 ) ) ;
#7828 = DIRECTION ( 'NONE',  ( 1.000000000000000000, 1.239088197126290570E-16, -0.000000000000000000 ) ) ;
#7829 = EDGE_CURVE ( 'NONE', #18169, #2733, #9452, .T. ) ;
#7830 = DIRECTION ( 'NONE',  ( -0.000000000000000000, -0.000000000000000000, -1.000000000000000000 ) ) ;
#7831 = DIRECTION ( 'NONE',  ( 0.000000000000000000, 0.000000000000000000, -1.000000000000000000 ) ) ;
#7832 = CARTESIAN_POINT ( 'NONE',  ( 1.321128355694181398E-14, -8.013167318348349610, 25.01316734529530095 ) ) ;
#7833 = CARTESIAN_POINT ( 'NONE',  ( 2.123976203522053297, -15.26039569100261950, 3.347755036805843076 ) ) ;
#7834 = EDGE_CURVE ( 'NONE', #4576, #12327, #3223, .T. ) ;
#7835 = ORIENTED_EDGE ( 'NONE', *, *, #14863, .F. ) ;
#7836 = AXIS2_PLACEMENT_3D ( 'NONE', #2534, #10989, #11170 ) ;
#7837 = VERTEX_POINT ( 'NONE', #3618 ) ;
#7838 = VECTOR ( 'NONE', #18284, 1000.000000000000000 ) ;
#7839 = ORIENTED_EDGE ( 'NONE', *, *, #1120, .T. ) ;
#7840 = ORIENTED_EDGE ( 'NONE', *, *, #16070, .T. ) ;
#7841 = CARTESIAN_POINT ( 'NONE',  ( 2.636624412716061627, -7.605649742761058540, -14.14563173255469408 ) ) ;
#7842 = CARTESIAN_POINT ( 'NONE',  ( 1.846955891736119293, 3.593597880662512623, -11.91257079808164576 ) ) ;
#7843 = CARTESIAN_POINT ( 'NONE',  ( -194.9999999999999716, -15.00000000000002665, 6.000000000000005329 ) ) ;
#7844 = DIRECTION ( 'NONE',  ( -0.5000000000000042188, 0.000000000000000000, 0.8660254037844361541 ) ) ;
#7845 = CARTESIAN_POINT ( 'NONE',  ( 0.4862570985993235340, 0.7479633556562450547, 13.89016912371017831 ) ) ;
#7846 = ORIENTED_EDGE ( 'NONE', *, *, #17215, .F. ) ;
#7847 = CARTESIAN_POINT ( 'NONE',  ( -4.195027931520234787, 7.500000000000000000, -16.53644619669688254 ) ) ;
#7848 = DIRECTION ( 'NONE',  ( 0.000000000000000000, -0.000000000000000000, -1.000000000000000000 ) ) ;
#7849 = VECTOR ( 'NONE', #10561, 1000.000000000000000 ) ;
#7850 = CARTESIAN_POINT ( 'NONE',  ( -1.876333640634785693, 7.499999999999999112, -15.16052078710835715 ) ) ;
#7851 = DIRECTION ( 'NONE',  ( -0.000000000000000000, 1.000000000000000000, 0.000000000000000000 ) ) ;
#7852 = CARTESIAN_POINT ( 'NONE',  ( 16.56872352241294521, -0.009382111268606286789, 0.004564908236400187953 ) ) ;
#7853 = CARTESIAN_POINT ( 'NONE',  ( 3.512766787570921867, 14.81029789862138912, 2.682019731918403593 ) ) ;
#7854 = DIRECTION ( 'NONE',  ( -0.000000000000000000, -1.000000000000000000, -0.000000000000000000 ) ) ;
#7855 = EDGE_CURVE ( 'NONE', #9430, #15279, #13556, .T. ) ;
#7856 = ADVANCED_FACE ( 'NONE', ( #2188 ), #3324, .T. ) ;
#7857 = ORIENTED_EDGE ( 'NONE', *, *, #10761, .F. ) ;
#7858 = AXIS2_PLACEMENT_3D ( 'NONE', #18611, #9642, #53 ) ;
#7859 = CARTESIAN_POINT ( 'NONE',  ( 2.320520222537155064, -14.32454429810361951, -6.542539914240126819 ) ) ;
#7861 = ORIENTED_EDGE ( 'NONE', *, *, #17410, .F. ) ;
#7860 = CARTESIAN_POINT ( 'NONE',  ( 1.846138399168762101, 11.95493567637855392, -3.446241763652874379 ) ) ;
#7862 = DIRECTION ( 'NONE',  ( -1.000000000000000000, -0.000000000000000000, -0.000000000000000000 ) ) ;
#7863 = VECTOR ( 'NONE', #4168, 1000.000000000000000 ) ;
#7864 = VECTOR ( 'NONE', #7023, 1000.000000000000000 ) ;
#7865 = CIRCLE ( 'NONE', #6328, 16.06066017081991149 ) ;
#7866 = VECTOR ( 'NONE', #17605, 1000.000000000000000 ) ;
#7867 = EDGE_LOOP ( 'NONE', ( #11990, #15210, #9971, #10064 ) ) ;
#7868 = LINE ( 'NONE', #13580, #6902 ) ;
#7869 = PRODUCT_DEFINITION_SHAPE ( 'NONE', 'NONE',  #18915 ) ;
#7870 = CARTESIAN_POINT ( 'NONE',  ( -0.06860918897761346391, -7.500000000000061284, -13.03178490627152186 ) ) ;
#7871 =( BOUNDED_SURFACE ( )  B_SPLINE_SURFACE ( 3, 1, ( 
 ( #12013, #6381 ),
 ( #6086, #353 ),
 ( #11916, #14877 ),
 ( #4654, #6182 ) ),
 .UNSPECIFIED., .F., .F., .T. ) 
 B_SPLINE_SURFACE_WITH_KNOTS ( ( 4, 4 ),
 ( 2, 2 ),
 ( 0.000000000000000000, 1.000000000000000000 ),
 ( 0.000000000000000000, 1.000000000000000000 ),
 .UNSPECIFIED. ) 
 GEOMETRIC_REPRESENTATION_ITEM ( )  RATIONAL_B_SPLINE_SURFACE ( (
 ( 1.000000000000000000, 1.000000000000000000),
 ( 0.9933953342250438912, 0.8357391271907739227),
 ( 0.9933953342250438912, 0.8357391271907739227),
 ( 1.000000000000000000, 1.000000000000000000) ) ) 
 REPRESENTATION_ITEM ( '' )  SURFACE ( )  );
#7872 = ORIENTED_EDGE ( 'NONE', *, *, #11705, .F. ) ;
#7873 = CARTESIAN_POINT ( 'NONE',  ( 2.747332970342022840, 7.555624153089857131, -14.49942876448584173 ) ) ;
#7874 = CARTESIAN_POINT ( 'NONE',  ( 8.522092701127531811, 4.388629235579577070, 5.397361180353158261 ) ) ;
#7875 = AXIS2_PLACEMENT_3D ( 'NONE', #15799, #4148, #7305 ) ;
#7876 = CARTESIAN_POINT ( 'NONE',  ( 0.8740779401508861346, -14.27348745891575987, 0.8420120399581260129 ) ) ;
#7877 = CARTESIAN_POINT ( 'NONE',  ( 2.320520222536476496, 15.64520721754621491, 1.795797593768047262 ) ) ;
#7878 = B_SPLINE_CURVE_WITH_KNOTS ( 'NONE', 3,
 ( #17089, #9809, #2542, #8391, #14222, #1122 ),
 .UNSPECIFIED., .F., .F.,
 ( 4, 2, 4 ),
 ( 0.000000000000000000, 0.001657017934709840989, 0.003314035869419681979 ),
 .UNSPECIFIED. ) ;
#7879 = VECTOR ( 'NONE', #12530, 1000.000000000000000 ) ;
#7880 = ORIENTED_EDGE ( 'NONE', *, *, #16283, .T. ) ;
#7881 = EDGE_CURVE ( 'NONE', #12842, #18304, #8025, .T. ) ;
#7882 = EDGE_CURVE ( 'NONE', #6956, #9697, #5958, .T. ) ;
#7883 = CARTESIAN_POINT ( 'NONE',  ( 2.002547531651519996, -4.532360870844247991, -11.75462648437106417 ) ) ;
#7884 = ADVANCED_FACE ( 'NONE', ( #8478 ), #2115, .F. ) ;
#7885 = CARTESIAN_POINT ( 'NONE',  ( 1.136128737974912818E-14, -7.013167318348350499, 27.61316734529538053 ) ) ;
#7887 = ORIENTED_EDGE ( 'NONE', *, *, #15281, .T. ) ;
#7886 = CARTESIAN_POINT ( 'NONE',  ( 12.00000000000000711, -19.99999999999999645, 3.000000000000000000 ) ) ;
#7888 = DIRECTION ( 'NONE',  ( -0.000000000000000000, -0.000000000000000000, 1.000000000000000000 ) ) ;
#7889 = AXIS2_PLACEMENT_3D ( 'NONE', #364, #6191, #16430 ) ;
#7890 = ORIENTED_EDGE ( 'NONE', *, *, #16782, .T. ) ;
#7891 = LINE ( 'NONE', #13701, #7392 ) ;
#7892 = DIRECTION ( 'NONE',  ( -1.000000000000000000, 0.000000000000000000, 0.000000000000000000 ) ) ;
#7893 = ORIENTED_EDGE ( 'NONE', *, *, #13574, .F. ) ;
#7894 = ORIENTED_EDGE ( 'NONE', *, *, #2025, .T. ) ;
#7895 = B_SPLINE_CURVE_WITH_KNOTS ( 'NONE', 3,
 ( #5536, #11482, #11577, #9838 ),
 .UNSPECIFIED., .F., .F.,
 ( 4, 4 ),
 ( 1.464275143509529362E-17, 0.003005512676784844427 ),
 .UNSPECIFIED. ) ;
#7896 = CARTESIAN_POINT ( 'NONE',  ( 0.3137051932979792457, 11.37800749014142276, -7.698472063774345564 ) ) ;
#7897 = ORIENTED_EDGE ( 'NONE', *, *, #17714, .F. ) ;
#7898 = CARTESIAN_POINT ( 'NONE',  ( 0.3720661004400040439, 11.58636699658215541, 7.524064345033506740 ) ) ;
#7899 = ORIENTED_EDGE ( 'NONE', *, *, #11190, .T. ) ;
#7900 = CARTESIAN_POINT ( 'NONE',  ( 3.074695600508088322, 15.41438262616131283, 2.093687500611883578 ) ) ;
#7901 = CARTESIAN_POINT ( 'NONE',  ( 0.3151926232592509591, -13.73922722301401400, 0.07678256780552859817 ) ) ;
#7902 = CARTESIAN_POINT ( 'NONE',  ( 12.00000000000000711, -14.99999999999999645, 3.000000000000000000 ) ) ;
#7903 = DIRECTION ( 'NONE',  ( 0.000000000000000000, 0.000000000000000000, 1.000000000000000000 ) ) ;
#7904 = AXIS2_PLACEMENT_3D ( 'NONE', #14860, #18871, #14473 ) ;
#7905 = CARTESIAN_POINT ( 'NONE',  ( 0.3308579732647025096, 12.88563776947746398, 4.812490080619245880 ) ) ;
#7906 = LINE ( 'NONE', #16679, #1381 ) ;
#7907 = CARTESIAN_POINT ( 'NONE',  ( 2.002547531651519996, -6.845637710436264456, 10.57595306287289638 ) ) ;
#7908 = CARTESIAN_POINT ( 'NONE',  ( -194.9999999999999716, -10.00000000000003020, 5.999999999999999112 ) ) ;
#7909 =( BOUNDED_SURFACE ( )  B_SPLINE_SURFACE ( 3, 1, ( 
 ( #14950, #16197 ),
 ( #431, #1483 ),
 ( #6261, #14566 ),
 ( #7319, #40 ) ),
 .UNSPECIFIED., .F., .F., .T. ) 
 B_SPLINE_SURFACE_WITH_KNOTS ( ( 4, 4 ),
 ( 2, 2 ),
 ( 0.000000000000000000, 1.000000000000000000 ),
 ( 0.000000000000000000, 1.000000000000000000 ),
 .UNSPECIFIED. ) 
 GEOMETRIC_REPRESENTATION_ITEM ( )  RATIONAL_B_SPLINE_SURFACE ( (
 ( 1.000000000000000000, 1.000000000000000000),
 ( 0.7792777138730160313, 0.9689936506012927220),
 ( 0.7792777138730160313, 0.9689936506012927220),
 ( 1.000000000000000000, 1.000000000000000000) ) ) 
 REPRESENTATION_ITEM ( '' )  SURFACE ( )  );
#7910 = CARTESIAN_POINT ( 'NONE',  ( 0.3058872367615230181, -8.562166468153638021, -10.75034008168925226 ) ) ;
#7911 = CARTESIAN_POINT ( 'NONE',  ( 3.377929128793386138, 13.92579934231094718, -1.296196549818984911 ) ) ;
#7912 = EDGE_CURVE ( 'NONE', #12351, #12889, #16476, .T. ) ;
#7913 = CARTESIAN_POINT ( 'NONE',  ( 0.3137051932979775248, 3.805684345189972895, -13.20008686438101719 ) ) ;
#7914 = DIRECTION ( 'NONE',  ( -1.000000000000000000, -0.000000000000000000, -0.000000000000000000 ) ) ;
#7915 = VERTEX_POINT ( 'NONE', #5500 ) ;
#7916 = ORIENTED_EDGE ( 'NONE', *, *, #10047, .T. ) ;
#7917 = EDGE_LOOP ( 'NONE', ( #3096, #16506, #17347, #3298 ) ) ;
#7918 = ORIENTED_EDGE ( 'NONE', *, *, #5587, .F. ) ;
#7919 = ORIENTED_EDGE ( 'NONE', *, *, #14022, .F. ) ;
#7920 = CARTESIAN_POINT ( 'NONE',  ( 0.4862570985993235340, 12.97920246947886191, -5.003653737315353567 ) ) ;
#7921 = CARTESIAN_POINT ( 'NONE',  ( 0.3720661004400037664, -7.524064345033377954, -11.58636699658223179 ) ) ;
#7922 = CARTESIAN_POINT ( 'NONE',  ( 1.959283090834839314, 9.750336807931262229, -7.909254450748897547 ) ) ;
#7923 = EDGE_CURVE ( 'NONE', #7190, #4602, #8471, .T. ) ;
#7924 = FACE_OUTER_BOUND ( 'NONE', #9519, .T. ) ;
#7925 = CARTESIAN_POINT ( 'NONE',  ( 2.320520222538070776, 1.795797593769018485, -15.64520721754711730 ) ) ;
#7926 = CARTESIAN_POINT ( 'NONE',  ( 0.4754618798421171855, 10.80499583390525764, -8.775436892860993154 ) ) ;
#7927 = CARTESIAN_POINT ( 'NONE',  ( 8.438534575730034959, 6.862570336891075762, 0.2320579683290369954 ) ) ;
#7928 = CARTESIAN_POINT ( 'NONE',  ( 2.636624412716061627, -7.605649742761058540, -14.14563173255469408 ) ) ;
#7929 = ADVANCED_FACE ( 'NONE', ( #18597 ), #7355, .F. ) ;
#7930 = ADVANCED_FACE ( 'NONE', ( #9721 ), #844, .T. ) ;
#7931 = CARTESIAN_POINT ( 'NONE',  ( 8.522092701127531811, -2.505958102592576342, -6.489356537178215589 ) ) ;
#7932 = ORIENTED_EDGE ( 'NONE', *, *, #2463, .T. ) ;
#7933 = ADVANCED_FACE ( 'NONE', ( #16892 ), #7180, .T. ) ;
#7934 = ORIENTED_EDGE ( 'NONE', *, *, #11937, .T. ) ;
#7935 = ORIENTED_EDGE ( 'NONE', *, *, #6491, .F. ) ;
#7936 =( REPRESENTATION_RELATIONSHIP ('NONE','NONE', #5200, #11674 ) REPRESENTATION_RELATIONSHIP_WITH_TRANSFORMATION ( #17318 )SHAPE_REPRESENTATION_RELATIONSHIP( ) );
#7937 = ORIENTED_EDGE ( 'NONE', *, *, #6846, .F. ) ;
#7938 = CARTESIAN_POINT ( 'NONE',  ( 8.438534575730034959, -3.845978796785994192, -5.688336279099088344 ) ) ;
#7939 = CARTESIAN_POINT ( 'NONE',  ( 2.002547531651519996, -0.6781519942172617998, 12.57989064830759318 ) ) ;
#7940 = CARTESIAN_POINT ( 'NONE',  ( 1.847412631396502913, -7.278870946904175909, -10.09191835241971269 ) ) ;
#7941 = LINE ( 'NONE', #12316, #6710 ) ;
#7942 = AXIS2_PLACEMENT_3D ( 'NONE', #13060, #4756, #12017 ) ;
#7943 = DIRECTION ( 'NONE',  ( 0.000000000000000000, -0.000000000000000000, -1.000000000000000000 ) ) ;
#7944 = ORIENTED_EDGE ( 'NONE', *, *, #6802, .T. ) ;
#7945 = AXIS2_PLACEMENT_3D ( 'NONE', #9747, #15300, #6614 ) ;
#7946 = CARTESIAN_POINT ( 'NONE',  ( 1.845755665166725068, -0.4784952423729416648, 12.43231320373360838 ) ) ;
#7947 = B_SPLINE_CURVE_WITH_KNOTS ( 'NONE', 3,
 ( #3803, #15553, #1021, #10993, #12501, #17086, #18247, #14115, #6863, #668, #8214, #3990, #5330 ),
 .UNSPECIFIED., .F., .F.,
 ( 4, 3, 3, 3, 4 ),
 ( 1.734723475976807094E-18, 0.0002299804304191480130, 0.0004599608082120234913, 0.0006467586077648008244, 0.0008336169836825994828 ),
 .UNSPECIFIED. ) ;
#7948 = EDGE_CURVE ( 'NONE', #9927, #7816, #16709, .T. ) ;
#7949 = CARTESIAN_POINT ( 'NONE',  ( 1.342453679581834924, -14.34050741580209198, 3.649820028552675844 ) ) ;
#7950 = CARTESIAN_POINT ( 'NONE',  ( -5.288115175735990547, 4.595214139557860733, -11.99999999743909740 ) ) ;
#7951 = CARTESIAN_POINT ( 'NONE',  ( 0.3058872367615230181, 12.87003593440634930, -4.821066432589193873 ) ) ;
#7952 = COLOUR_RGB ( '', 0.66274510, 0.83137255, 0.94901961) ;
#7953 = DIRECTION ( 'NONE',  ( -1.000000000000000000, -0.000000000000000000, -0.000000000000000000 ) ) ;
#7954 = ADVANCED_FACE ( 'NONE', ( #12679 ), #16988, .T. ) ;
#7955 = CARTESIAN_POINT ( 'NONE',  ( 3.950837973638668288, 0.000000000000000000, 0.000000000000000000 ) ) ;
#7956 = CARTESIAN_POINT ( 'NONE',  ( 0.4862570985993235340, 0.7479633556564388996, -13.89016912371016765 ) ) ;
#7957 = ORIENTED_EDGE ( 'NONE', *, *, #9685, .T. ) ;
#7959 = ORIENTED_EDGE ( 'NONE', *, *, #18629, .T. ) ;
#7958 = CARTESIAN_POINT ( 'NONE',  ( 6.000000000000001776, 17.00000000000000000, 3.000000000000000000 ) ) ;
#7960 = DIRECTION ( 'NONE',  ( 0.000000000000000000, 0.000000000000000000, 1.000000000000000000 ) ) ;
#7961 = ORIENTED_EDGE ( 'NONE', *, *, #3153, .F. ) ;
#7962 = CARTESIAN_POINT ( 'NONE',  ( 3.664313757352976708, 5.926151963190554817, -12.97355833021534011 ) ) ;
#7963 = CARTESIAN_POINT ( 'NONE',  ( -3.324307330593659238, -6.179741886604213974, -11.99999999169353160 ) ) ;
#7964 = ORIENTED_EDGE ( 'NONE', *, *, #15446, .F. ) ;
#7965 = CARTESIAN_POINT ( 'NONE',  ( 1.846613052777651198, 3.520031056876471887, -11.93415846513958023 ) ) ;
#7966 = EDGE_CURVE ( 'NONE', #3343, #5504, #15454, .T. ) ;
#7967 = CARTESIAN_POINT ( 'NONE',  ( 3.377929128793398128, 7.136734442941011558, -12.02809354424093691 ) ) ;
#7968 = CARTESIAN_POINT ( 'NONE',  ( 0.4862570985993235340, -8.769551628660655851, -10.79774104611382946 ) ) ;
#7969 = CARTESIAN_POINT ( 'NONE',  ( 2.002547531651519996, 7.942910686618173344, 9.778737580845726640 ) ) ;
#7970 = SURFACE_SIDE_STYLE ('',( #16747 ) ) ;
#7971 = CARTESIAN_POINT ( 'NONE',  ( 0.3137051932979792457, 11.37800749014142276, -7.698472063774345564 ) ) ;
#7972 = FACE_OUTER_BOUND ( 'NONE', #10721, .T. ) ;
#7974 = ORIENTED_EDGE ( 'NONE', *, *, #2909, .T. ) ;
#7973 = CARTESIAN_POINT ( 'NONE',  ( 1.845755665166725068, 10.33920510797153369, -6.920419570228236950 ) ) ;
#7975 = CARTESIAN_POINT ( 'NONE',  ( 2.002547531651520885, -4.532360870844412304, 11.75462648437100377 ) ) ;
#7976 = B_SPLINE_CURVE_WITH_KNOTS ( 'NONE', 3,
 ( #13079, #15755, #5708, #4105 ),
 .UNSPECIFIED., .F., .F.,
 ( 4, 4 ),
 ( 0.000000000000000000, 0.002004993803842769744 ),
 .UNSPECIFIED. ) ;
#7977 = EDGE_LOOP ( 'NONE', ( #15297, #14017, #1367, #13082 ) ) ;
#7978 = CARTESIAN_POINT ( 'NONE',  ( 2.320520222537280297, -15.64520721754692190, -1.795797593768913236 ) ) ;
#7979 = CARTESIAN_POINT ( 'NONE',  ( 1.861706995891668326, 11.66987142852990189, -4.359009869687124450 ) ) ;
#7980 =( BOUNDED_SURFACE ( )  B_SPLINE_SURFACE ( 3, 1, ( 
 ( #15044, #10461 ),
 ( #13614, #16103 ),
 ( #6260, #9029 ),
 ( #1766, #7610 ) ),
 .UNSPECIFIED., .F., .F., .T. ) 
 B_SPLINE_SURFACE_WITH_KNOTS ( ( 4, 4 ),
 ( 2, 2 ),
 ( 0.000000000000000000, 1.000000000000000000 ),
 ( 0.000000000000000000, 1.000000000000000000 ),
 .UNSPECIFIED. ) 
 GEOMETRIC_REPRESENTATION_ITEM ( )  RATIONAL_B_SPLINE_SURFACE ( (
 ( 1.000000000000000000, 1.000000000000000000),
 ( 0.9593108457356467333, 0.9995965569486454649),
 ( 0.9593108457356467333, 0.9995965569486454649),
 ( 1.000000000000000000, 1.000000000000000000) ) ) 
 REPRESENTATION_ITEM ( '' )  SURFACE ( )  );
#7981 = ORIENTED_EDGE ( 'NONE', *, *, #15527, .T. ) ;
#7982 = ORIENTED_EDGE ( 'NONE', *, *, #11782, .F. ) ;
#7983 = DIRECTION ( 'NONE',  ( -0.9034263296138832500, 0.000000000000000000, -0.4287433579198481337 ) ) ;
#7984 = CARTESIAN_POINT ( 'NONE',  ( 8.522092701127531811, -6.946128462138593029, -0.3779863304871954321 ) ) ;
#7985 = ORIENTED_EDGE ( 'NONE', *, *, #6091, .T. ) ;
#7986 = EDGE_CURVE ( 'NONE', #12607, #17875, #8206, .T. ) ;
#7987 = ADVANCED_FACE ( 'NONE', ( #12581 ), #18410, .T. ) ;
#7988 = ADVANCED_FACE ( 'NONE', ( #4460, #7242, #3101, #17260 ), #7432, .F. ) ;
#7989 = VECTOR ( 'NONE', #3505, 1000.000000000000227 ) ;
#7990 = LINE ( 'NONE', #6643, #11612 ) ;
#7991 = DIRECTION ( 'NONE',  ( -1.000000000000000000, 0.000000000000000000, 0.000000000000000000 ) ) ;
#7992 = CARTESIAN_POINT ( 'NONE',  ( 0.3132635586635976188, -7.641727604903970850, 11.41586812343486912 ) ) ;
#7993 = CARTESIAN_POINT ( 'NONE',  ( 0.3095370825347234511, -3.806662003783320980, -13.20347358821918426 ) ) ;
#7994 = APPLICATION_PROTOCOL_DEFINITION ( 'draft international standard', 'automotive_design', 1998, #3750 ) ;
#7995 = CARTESIAN_POINT ( 'NONE',  ( 3.353306896162455697, 13.88482890973696726, 1.348936822032873240 ) ) ;
#7996 = CARTESIAN_POINT ( 'NONE',  ( 2.320520222538103638, 6.542539914241700671, -14.32454429810417906 ) ) ;
#7997 = CARTESIAN_POINT ( 'NONE',  ( 0.4754618798421162973, -12.98792082933648118, 5.007009103465200894 ) ) ;
#7998 = CARTESIAN_POINT ( 'NONE',  ( 2.002547531651519996, -6.845637710436110801, -10.57595306287299763 ) ) ;
#7999 = VECTOR ( 'NONE', #2038, 1000.000000000000000 ) ;
#8000 = DIRECTION ( 'NONE',  ( -1.000000000000000000, 0.000000000000000000, -0.000000000000000000 ) ) ;
#8001 = CARTESIAN_POINT ( 'NONE',  ( 16.58200780006414732, -0.01041078477703985539, 0.004047297414157853025 ) ) ;
#8002 = ORIENTED_EDGE ( 'NONE', *, *, #7420, .F. ) ;
#8003 = EDGE_LOOP ( 'NONE', ( #8569, #5988, #18525, #8850 ) ) ;
#8004 = VERTEX_POINT ( 'NONE', #5986 ) ;
#8005 = ORIENTED_EDGE ( 'NONE', *, *, #17474, .T. ) ;
#8006 = DIRECTION ( 'NONE',  ( -1.000000000000000000, 0.000000000000000000, 0.000000000000000000 ) ) ;
#8007 = DIRECTION ( 'NONE',  ( -1.000000000000000000, 0.000000000000000000, 0.000000000000000000 ) ) ;
#8008 = ADVANCED_FACE ( 'NONE', ( #18882 ), #8564, .F. ) ;
#8009 = CARTESIAN_POINT ( 'NONE',  ( 1.342453679581834924, 7.902645620902447376, 12.51077660954468662 ) ) ;
#8010 = CARTESIAN_POINT ( 'NONE',  ( 1.847247051441591514, -11.88474976472815214, 3.685275815977142599 ) ) ;
#8011 = DIRECTION ( 'NONE',  ( 0.000000000000000000, 0.000000000000000000, -1.000000000000000000 ) ) ;
#8012 = DIRECTION ( 'NONE',  ( 1.000000000000000000, 0.000000000000000000, 0.000000000000000000 ) ) ;
#8013 = CARTESIAN_POINT ( 'NONE',  ( 3.950837973638675393, -14.31366178983251380, -2.591948120961955926 ) ) ;
#8014 = VECTOR ( 'NONE', #11191, 1000.000000000000000 ) ;
#8015 = CARTESIAN_POINT ( 'NONE',  ( -61.35602477868047799, -15.00000000000001066, 6.000000000000005329 ) ) ;
#8016 = CARTESIAN_POINT ( 'NONE',  ( 3.950837973638675393, 2.591948120961804936, 14.31366178983254578 ) ) ;
#8017 = EDGE_CURVE ( 'NONE', #18680, #10243, #4273, .T. ) ;
#8018 = EDGE_LOOP ( 'NONE', ( #10777, #14650, #16824, #16092 ) ) ;
#8019 = B_SPLINE_CURVE_WITH_KNOTS ( 'NONE', 3,
 ( #18774, #5488, #15815, #15531 ),
 .UNSPECIFIED., .F., .F.,
 ( 4, 4 ),
 ( 1.811104479740059440E-17, 0.003005512676784850932 ),
 .UNSPECIFIED. ) ;
#8020 = ORIENTED_EDGE ( 'NONE', *, *, #6641, .F. ) ;
#8021 = VERTEX_POINT ( 'NONE', #2722 ) ;
#8022 = ORIENTED_EDGE ( 'NONE', *, *, #5472, .F. ) ;
#8023 = DIRECTION ( 'NONE',  ( 0.000000000000000000, 0.000000000000000000, 1.000000000000000000 ) ) ;
#8024 = CARTESIAN_POINT ( 'NONE',  ( 2.949999999999999734, 0.000000000000000000, 2.499999999999999556 ) ) ;
#8025 = LINE ( 'NONE', #7843, #6569 ) ;
#8026 = CARTESIAN_POINT ( 'NONE',  ( 16.57210152137263393, -0.005118120558002011225, -0.01361613799508959964 ) ) ;
#8027 = AXIS2_PLACEMENT_3D ( 'NONE', #15903, #14286, #9974 ) ;
#8028 = EDGE_CURVE ( 'NONE', #622, #18897, #14194, .T. ) ;
#8029 = DIRECTION ( 'NONE',  ( 0.000000000000000000, 0.000000000000000000, 1.000000000000000000 ) ) ;
#8030 = EDGE_LOOP ( 'NONE', ( #4057, #13435, #16445, #17946 ) ) ;
#8031 = CARTESIAN_POINT ( 'NONE',  ( 2.123976203522053297, -11.67822624909917550, -10.37815841598504107 ) ) ;
#8032 = DIRECTION ( 'NONE',  ( -0.7561779333270775005, 0.5491072561318340872, 0.3559159372837335522 ) ) ;
#8033 = EDGE_CURVE ( 'NONE', #617, #15501, #14627, .T. ) ;
#8034 = ADVANCED_FACE ( 'NONE', ( #4560 ), #9301, .F. ) ;
#8035 = CARTESIAN_POINT ( 'NONE',  ( -4.227723179941619058, 5.599337756632279728, -12.00000000790602428 ) ) ;
#8036 = CARTESIAN_POINT ( 'NONE',  ( -27.32408120756002035, 15.00000000000000000, 0.000000000000000000 ) ) ;
#8037 = DIRECTION ( 'NONE',  ( -0.000000000000000000, -0.000000000000000000, -1.000000000000000000 ) ) ;
#8038 = CARTESIAN_POINT ( 'NONE',  ( 1.846138399168762989, 11.95493567637850774, 3.446241763653039580 ) ) ;
#8039 = CARTESIAN_POINT ( 'NONE',  ( -194.9999999999999716, -5.000000000000024869, 3.000000000000002665 ) ) ;
#8040 = CARTESIAN_POINT ( 'NONE',  ( 0.3137051932979792457, 11.37800749014131263, 7.698472063774513430 ) ) ;
#8041 = ORIENTED_EDGE ( 'NONE', *, *, #12824, .F. ) ;
#8042 = APPLICATION_CONTEXT ( 'automotive_design' ) ;
#8044 = EDGE_LOOP ( 'NONE', ( #14655, #12180 ) ) ;
#8043 = CARTESIAN_POINT ( 'NONE',  ( 1.847247051441592625, 11.88474976472817701, -3.685275815977066216 ) ) ;
#8045 = CARTESIAN_POINT ( 'NONE',  ( 16.56822296793089322, 0.0007467251401288622394, -0.01011126603341004279 ) ) ;
#8046 = EDGE_CURVE ( 'NONE', #18780, #13920, #10862, .T. ) ;
#8047 = AXIS2_PLACEMENT_3D ( 'NONE', #1461, #1360, #7103 ) ;
#8048 = VERTEX_POINT ( 'NONE', #13347 ) ;
#8049 = CARTESIAN_POINT ( 'NONE',  ( 0.3095370825347233956, 11.38092634279628967, 7.700448427571912724 ) ) ;
#8050 = B_SPLINE_CURVE_WITH_KNOTS ( 'NONE', 3,
 ( #7845, #13666, #9167, #14900, #6307, #15193 ),
 .UNSPECIFIED., .F., .F.,
 ( 4, 2, 4 ),
 ( 5.421010862427522170E-20, 0.001657017934710529891, 0.003314035869421059783 ),
 .UNSPECIFIED. ) ;
#8051 = CARTESIAN_POINT ( 'NONE',  ( -0.6925461861254285090, -7.500000000000000888, -14.36265820198516074 ) ) ;
#8052 = ORIENTED_EDGE ( 'NONE', *, *, #13261, .T. ) ;
#8053 = DIRECTION ( 'NONE',  ( -0.000000000000000000, 1.000000000000000000, -0.000000000000000000 ) ) ;
#8054 = DIRECTION ( 'NONE',  ( 0.000000000000000000, 0.000000000000000000, 1.000000000000000000 ) ) ;
#8055 = CARTESIAN_POINT ( 'NONE',  ( 0.4862570985993235340, -13.89016912371018186, 0.7479633556561964269 ) ) ;
#8056 = FACE_OUTER_BOUND ( 'NONE', #3594, .T. ) ;
#8057 = B_SPLINE_CURVE_WITH_KNOTS ( 'NONE', 3,
 ( #4971, #8220, #13674, #10806, #16632, #6503 ),
 .UNSPECIFIED., .F., .F.,
 ( 4, 2, 4 ),
 ( 9.263427422397552964E-19, 0.001500839035891552656, 0.003001678071783104446 ),
 .UNSPECIFIED. ) ;
#8058 = VECTOR ( 'NONE', #18724, 1000.000000000000114 ) ;
#8059 = EDGE_CURVE ( 'NONE', #2148, #1614, #8938, .T. ) ;
#8060 = CARTESIAN_POINT ( 'NONE',  ( 0.3137051932979809665, 13.20008686438111312, -3.805684345189650042 ) ) ;
#8061 = LINE ( 'NONE', #6529, #6156 ) ;
#8063 = ORIENTED_EDGE ( 'NONE', *, *, #18182, .T. ) ;
#8062 = DIRECTION ( 'NONE',  ( 0.000000000000000000, 0.000000000000000000, 1.000000000000000000 ) ) ;
#8064 = CARTESIAN_POINT ( 'NONE',  ( -194.9999999999999716, -5.000000000000024869, 6.000000000000000000 ) ) ;
#8065 = EDGE_CURVE ( 'NONE', #14465, #16063, #4137, .T. ) ;
#8066 = VERTEX_POINT ( 'NONE', #8657 ) ;
#8067 = LINE ( 'NONE', #13875, #9526 ) ;
#8068 = CARTESIAN_POINT ( 'NONE',  ( 1.918918678667046240, 11.69059232068584819, -4.466049546133788795 ) ) ;
#8069 = VERTEX_POINT ( 'NONE', #4364 ) ;
#8070 = B_SPLINE_CURVE_WITH_KNOTS ( 'NONE', 3,
 ( #16882, #10885, #6763, #6215, #13824, #9443 ),
 .UNSPECIFIED., .F., .F.,
 ( 4, 2, 4 ),
 ( 4.027530160694267299E-17, 0.0002014099069817290014, 0.0004028198139634177246 ),
 .UNSPECIFIED. ) ;
#8071 = ORIENTED_EDGE ( 'NONE', *, *, #16025, .F. ) ;
#8072 = CARTESIAN_POINT ( 'NONE',  ( 1.861706995891668104, -9.751699138048492088, 7.751853334747282886 ) ) ;
#8073 = CARTESIAN_POINT ( 'NONE',  ( 16.56872352241294521, -0.001442253899401880124, -0.01033355228142401362 ) ) ;
#8074 = VERTEX_POINT ( 'NONE', #61 ) ;
#8075 = AXIS2_PLACEMENT_3D ( 'NONE', #14705, #6989, #4388 ) ;
#8076 = CIRCLE ( 'NONE', #2261, 12.15840553252917289 ) ;
#8077 = PRODUCT_DEFINITION_FORMATION_WITH_SPECIFIED_SOURCE ( 'ANY', '', #684, .NOT_KNOWN. ) ;
#8078 = DIRECTION ( 'NONE',  ( -0.000000000000000000, 1.000000000000000000, -0.000000000000000000 ) ) ;
#8079 = CARTESIAN_POINT ( 'NONE',  ( 0.4754618798421171855, 12.98792082933651493, -5.007009103465112076 ) ) ;
#8080 = CARTESIAN_POINT ( 'NONE',  ( 16.56872352241294521, -0.004907101719994693724, 0.009207754980063731845 ) ) ;
#8081 = CARTESIAN_POINT ( 'NONE',  ( 2.636624412717099908, 11.60464335004051861, -11.10302021258208249 ) ) ;
#8082 =( BOUNDED_SURFACE ( )  B_SPLINE_SURFACE ( 3, 1, ( 
 ( #6629, #16936 ),
 ( #8158, #10741 ),
 ( #13973, #15498 ),
 ( #2141, #18280 ) ),
 .UNSPECIFIED., .F., .F., .T. ) 
 B_SPLINE_SURFACE_WITH_KNOTS ( ( 4, 4 ),
 ( 2, 2 ),
 ( 0.000000000000000000, 1.000000000000000000 ),
 ( 0.000000000000000000, 1.000000000000000000 ),
 .UNSPECIFIED. ) 
 GEOMETRIC_REPRESENTATION_ITEM ( )  RATIONAL_B_SPLINE_SURFACE ( (
 ( 1.000000000000000000, 1.000000000000000000),
 ( 0.7792777138730158093, 0.9689936506012928330),
 ( 0.7792777138730158093, 0.9689936506012928330),
 ( 1.000000000000000000, 1.000000000000000000) ) ) 
 REPRESENTATION_ITEM ( '' )  SURFACE ( )  );
#8083 = CARTESIAN_POINT ( 'NONE',  ( 1.451356985208878270E-14, -7.013167318348350499, 33.78111653772643308 ) ) ;
#8084 = CARTESIAN_POINT ( 'NONE',  ( 4.336808689942017736E-15, -30.00000000000000000, 26.00000000000000000 ) ) ;
#8085 = EDGE_CURVE ( 'NONE', #10095, #14563, #8853, .T. ) ;
#8086 = EDGE_CURVE ( 'NONE', #15500, #5687, #6880, .T. ) ;
#8087 = EDGE_CURVE ( 'NONE', #3366, #16117, #13437, .T. ) ;
#8088 = VECTOR ( 'NONE', #17577, 1000.000000000000114 ) ;
#8089 = CARTESIAN_POINT ( 'NONE',  ( 0.3939875929385656117, -13.34133634968952720, -3.598491969338368346 ) ) ;
#8090 = CARTESIAN_POINT ( 'NONE',  ( 2.949999999999999734, 0.000000000000000000, 0.000000000000000000 ) ) ;
#8091 = ORIENTED_EDGE ( 'NONE', *, *, #9260, .T. ) ;
#8092 = VERTEX_POINT ( 'NONE', #1981 ) ;
#8093 = B_SPLINE_CURVE_WITH_KNOTS ( 'NONE', 3,
 ( #4370, #18890, #2640, #1212, #5597, #11545, #7057, #5790, #11636, #10003, #2818, #17364, #4280 ),
 .UNSPECIFIED., .F., .F.,
 ( 4, 3, 3, 3, 4 ),
 ( 3.878959614448864246E-18, 0.0002299780670421063358, 0.0004599561239687880061, 0.0006896788984287903403, 0.0009194956271626402800 ),
 .UNSPECIFIED. ) ;
#8094 = ORIENTED_EDGE ( 'NONE', *, *, #12513, .F. ) ;
#8095 = VERTEX_POINT ( 'NONE', #16420 ) ;
#8096 = CARTESIAN_POINT ( 'NONE',  ( 0.4384471787762818096, 0.7363690479466327155, 13.84291427302852462 ) ) ;
#8097 = CARTESIAN_POINT ( 'NONE',  ( 0.4754618798421162973, -7.564402563418381575, -11.68486377711974811 ) ) ;
#8098 = AXIS2_PLACEMENT_3D ( 'NONE', #1503, #10096, #11268 ) ;
#8099 = VERTEX_POINT ( 'NONE', #16512 ) ;
#8100 = LINE ( 'NONE', #646, #1369 ) ;
#8101 = LINE ( 'NONE', #12301, #16206 ) ;
#8102 = VECTOR ( 'NONE', #17735, 1000.000000000000000 ) ;
#8103 = B_SPLINE_CURVE_WITH_KNOTS ( 'NONE', 3,
 ( #17669, #14976, #16328, #11832, #12124, #13160, #4759, #17562, #12023, #4372 ),
 .UNSPECIFIED., .F., .F.,
 ( 4, 3, 3, 4 ),
 ( 0.0004168119862248656667, 0.0004599608082120252802, 0.0006467586077648016917, 0.0008336169836825988323 ),
 .UNSPECIFIED. ) ;
#8104 = CIRCLE ( 'NONE', #17235, 2.749999999999998224 ) ;
#8105 = CARTESIAN_POINT ( 'NONE',  ( 0.3095370825347233956, 10.84046130709070610, -8.444334731363889901 ) ) ;
#8106 = FACE_OUTER_BOUND ( 'NONE', #13413, .T. ) ;
#8107 = EDGE_CURVE ( 'NONE', #879, #12951, #10480, .T. ) ;
#8108 = CARTESIAN_POINT ( 'NONE',  ( 0.3095370825347224519, -3.806662003783324089, -13.20347358821918249 ) ) ;
#8109 = CARTESIAN_POINT ( 'NONE',  ( 3.512766787570764215, -6.535475144497081779, 13.55823433651946175 ) ) ;
#8110 = ORIENTED_EDGE ( 'NONE', *, *, #13914, .T. ) ;
#8111 = ADVANCED_FACE ( 'NONE', ( #16317 ), #11760, .F. ) ;
#8112 = ORIENTED_EDGE ( 'NONE', *, *, #18263, .T. ) ;
#8113 = ORIENTED_EDGE ( 'NONE', *, *, #17820, .F. ) ;
#8114 = ADVANCED_FACE ( 'NONE', ( #4848 ), #1788, .F. ) ;
#8115 = AXIS2_PLACEMENT_3D ( 'NONE', #16373, #16469, #7485 ) ;
#8116 = VERTEX_POINT ( 'NONE', #10584 ) ;
#8117 = AXIS2_PLACEMENT_3D ( 'NONE', #13758, #673, #12241 ) ;
#8118 = CARTESIAN_POINT ( 'NONE',  ( -6.000000000000000888, 17.00000000000000000, 3.000000000000000000 ) ) ;
#8119 = CARTESIAN_POINT ( 'NONE',  ( 0.000000000000000000, 0.000000000000000000, 0.000000000000000000 ) ) ;
#8120 = CARTESIAN_POINT ( 'NONE',  ( 16.56822296793089322, 0.005339139727952666586, -0.008619100080559792543 ) ) ;
#8121 = CARTESIAN_POINT ( 'NONE',  ( 1.846138399168762101, 12.43476674860266584, 0.4167076046095977149 ) ) ;
#8122 = CARTESIAN_POINT ( 'NONE',  ( 16.56872352241294521, -0.001821578298044716857, -0.01027347319884440967 ) ) ;
#8123 = VERTEX_POINT ( 'NONE', #15064 ) ;
#8124 = CARTESIAN_POINT ( 'NONE',  ( 16.56872352241294521, 0.001821578298044641397, 0.01027347319884442528 ) ) ;
#8125 = CARTESIAN_POINT ( 'NONE',  ( 0.3939822652208137543, 11.57634296752778802, -7.545099438011897419 ) ) ;
#8126 = CARTESIAN_POINT ( 'NONE',  ( -5.872941918984155407, 7.499999999999997335, -12.71526091932764224 ) ) ;
#8127 = CARTESIAN_POINT ( 'NONE',  ( 2.320520222538102306, -7.743191299716920106, -13.71278186123380927 ) ) ;
#8128 = CARTESIAN_POINT ( 'NONE',  ( 0.000000000000000000, 0.000000000000000000, 3.000000000000000000 ) ) ;
#8129 = DIRECTION ( 'NONE',  ( 0.000000000000000000, 0.000000000000000000, 1.000000000000000000 ) ) ;
#8130 = CARTESIAN_POINT ( 'NONE',  ( 2.750000000000000000, 5.817072295949927426E-16, -4.750000000000000000 ) ) ;
#8131 = MECHANICAL_DESIGN_GEOMETRIC_PRESENTATION_REPRESENTATION (  '', ( #3844 ), #1719 ) ;
#8132 = CARTESIAN_POINT ( 'NONE',  ( 1.918921323896325193, -4.466082741316288462, 11.69058285425789201 ) ) ;
#8133 = EDGE_LOOP ( 'NONE', ( #15633, #17277 ) ) ;
#8134 = VERTEX_POINT ( 'NONE', #555 ) ;
#8135 = FACE_OUTER_BOUND ( 'NONE', #4156, .T. ) ;
#8136 = ADVANCED_FACE ( 'NONE', ( #9047 ), #7871, .F. ) ;
#8137 = FACE_OUTER_BOUND ( 'NONE', #18502, .T. ) ;
#8138 = VERTEX_POINT ( 'NONE', #3303 ) ;
#8139 = CARTESIAN_POINT ( 'NONE',  ( 1.846822687350019310, -3.566003975885607691, -11.92063725419902731 ) ) ;
#8140 = CIRCLE ( 'NONE', #806, 14.54644660717763927 ) ;
#8141 = CARTESIAN_POINT ( 'NONE',  ( -3.606670283718027559, -7.500000000000000888, -16.27044756620548327 ) ) ;
#8142 = PRESENTATION_LAYER_ASSIGNMENT (  '', '', ( #18214 ) ) ;
#8143 = VERTEX_POINT ( 'NONE', #14966 ) ;
#8144 = LINE ( 'NONE', #869, #1984 ) ;
#8145 = CARTESIAN_POINT ( 'NONE',  ( 0.4862570985993235340, 3.580942890621860109, -13.44146924561377254 ) ) ;
#8146 = DIRECTION ( 'NONE',  ( 0.7635533937278216055, 0.6453904417649386493, 0.02138673900302558509 ) ) ;
#8147 = FACE_OUTER_BOUND ( 'NONE', #4222, .T. ) ;
#8148 = ADVANCED_FACE ( 'NONE', ( #1886 ), #6001, .F. ) ;
#8149 = VECTOR ( 'NONE', #6698, 1000.000000000000000 ) ;
#8150 = CARTESIAN_POINT ( 'NONE',  ( 1.254009781011991898, 3.563484327698415388, -14.24044713813362151 ) ) ;
#8151 = AXIS2_PLACEMENT_3D ( 'NONE', #3212, #17296, #16431 ) ;
#8152 = CARTESIAN_POINT ( 'NONE',  ( 0.3170788640506440603, 8.200855617524691610, -11.02668139258432944 ) ) ;
#8154 = ORIENTED_EDGE ( 'NONE', *, *, #567, .F. ) ;
#8153 = FACE_OUTER_BOUND ( 'NONE', #17141, .T. ) ;
#8155 = CARTESIAN_POINT ( 'NONE',  ( 0.000000000000000000, 0.000000000000000000, 6.000000000000000000 ) ) ;
#8156 = VECTOR ( 'NONE', #16585, 1000.000000000000000 ) ;
#8157 = CARTESIAN_POINT ( 'NONE',  ( 16.56679352167444819, -0.004277682826582317882, 0.008252760440870482092 ) ) ;
#8158 = CARTESIAN_POINT ( 'NONE',  ( 16.57778382496167424, -0.01482878558584568157, -0.001819584982832054632 ) ) ;
#8159 = CARTESIAN_POINT ( 'NONE',  ( 0.3142014840576518586, -3.879477880151352753, -13.17932813834298678 ) ) ;
#8160 = ORIENTED_EDGE ( 'NONE', *, *, #7882, .F. ) ;
#8161 = ORIENTED_EDGE ( 'NONE', *, *, #5261, .T. ) ;
#8162 = CARTESIAN_POINT ( 'NONE',  ( 2.636624412715137922, 2.161493821597615828, 15.91454522070216093 ) ) ;
#8163 = CIRCLE ( 'NONE', #18823, 2.600000000000092015 ) ;
#8164 = FACE_OUTER_BOUND ( 'NONE', #12701, .T. ) ;
#8165 = ORIENTED_EDGE ( 'NONE', *, *, #3779, .T. ) ;
#8166 = CIRCLE ( 'NONE', #9969, 2.499999999999999556 ) ;
#8167 = CARTESIAN_POINT ( 'NONE',  ( 0.4754618798421171855, -0.7484603771383426807, -13.89949764182683545 ) ) ;
#8168 = EDGE_CURVE ( 'NONE', #9866, #6897, #10303, .T. ) ;
#8169 = STYLED_ITEM ( 'NONE', ( #16396 ), #16668 ) ;
#8170 = CARTESIAN_POINT ( 'NONE',  ( 1.847168016377985111, -10.17509564929253507, -7.161712042621569019 ) ) ;
#8171 = CLOSED_SHELL ( 'NONE', ( #13610, #1637, #16651, #2441, #4284, #6093, #16758, #5909, #17703, #5803, #14103, #8784, #15299, #4235, #18490, #2246, #14625, #14623, #1229, #1844, #7499, #10017, #11875, #17409, #13290, #6004, #2392, #2154, #9963, #9740, #1026, #17408, #7618, #6851, #1955, #5883, #9438 ) ) ;
#8172 = CARTESIAN_POINT ( 'NONE',  ( 1.861628059977341598, 12.44564375541077617, 0.5393144007390715533 ) ) ;
#8173 = DIRECTION ( 'NONE',  ( -1.000000000000000000, -0.000000000000000000, -0.000000000000000000 ) ) ;
#8174 = PRODUCT_CONTEXT ( 'NONE', #6695, 'mechanical' ) ;
#8175 = LINE ( 'NONE', #4043, #4977 ) ;
#8176 = EDGE_CURVE ( 'NONE', #9741, #748, #11469, .T. ) ;
#8177 = DIRECTION ( 'NONE',  ( -1.000000000000000000, -0.000000000000000000, -0.000000000000000000 ) ) ;
#8178 = CARTESIAN_POINT ( 'NONE',  ( 0.3307726912345191894, -4.812300915532890855, -12.88561780039863436 ) ) ;
#8179 = CARTESIAN_POINT ( 'NONE',  ( 16.56679352167444819, -0.001390132774595520624, -0.009190982326619362083 ) ) ;
#8180 = CARTESIAN_POINT ( 'NONE',  ( 2.636624412716062071, -14.14563173255412742, -7.605649742760987486 ) ) ;
#8181 = CARTESIAN_POINT ( 'NONE',  ( 16.56753206892534891, 0.006760771273035115839, -0.006669401563385219701 ) ) ;
#8182 = ORIENTED_EDGE ( 'NONE', *, *, #1790, .F. ) ;
#8183 = ORIENTED_EDGE ( 'NONE', *, *, #847, .T. ) ;
#8184 = ORIENTED_EDGE ( 'NONE', *, *, #10894, .T. ) ;
#8185 = ORIENTED_EDGE ( 'NONE', *, *, #10971, .F. ) ;
#8186 = EDGE_LOOP ( 'NONE', ( #2078, #12409, #2652, #7000 ) ) ;
#8187 = VECTOR ( 'NONE', #17538, 1000.000000000000000 ) ;
#8188 = DIRECTION ( 'NONE',  ( 1.000000000000000000, 0.000000000000000000, -0.000000000000000000 ) ) ;
#8189 = EDGE_CURVE ( 'NONE', #16119, #13313, #1428, .T. ) ;
#8190 = CARTESIAN_POINT ( 'NONE',  ( -3.337222544067827368, -7.500000000000000888, -16.12749921823413146 ) ) ;
#8191 = ADVANCED_FACE ( 'NONE', ( #7268 ), #16146, .F. ) ;
#8192 = CARTESIAN_POINT ( 'NONE',  ( 2.002547531651519996, 6.845637710436190737, 10.57595306287294612 ) ) ;
#8193 = CARTESIAN_POINT ( 'NONE',  ( 1.845755665166725068, 6.920419570228353301, 10.33920510797145909 ) ) ;
#8194 = CARTESIAN_POINT ( 'NONE',  ( 16.58200780006414732, -0.0006320991582339893951, -0.01115192838421470191 ) ) ;
#8195 = CARTESIAN_POINT ( 'NONE',  ( -59.99999999999997158, -25.00000000000000711, 0.000000000000000000 ) ) ;
#8196 = CARTESIAN_POINT ( 'NONE',  ( 3.950837973638677170, 1.958075594453790869, 14.41405733518061538 ) ) ;
#8197 = FACE_OUTER_BOUND ( 'NONE', #7028, .T. ) ;
#8198 = CARTESIAN_POINT ( 'NONE',  ( 0.4754618798421167414, -13.45049478164062329, 3.583352865732619463 ) ) ;
#8199 = ORIENTED_EDGE ( 'NONE', *, *, #3890, .T. ) ;
#8200 = ORIENTED_EDGE ( 'NONE', *, *, #10608, .F. ) ;
#8201 = B_SPLINE_CURVE_WITH_KNOTS ( 'NONE', 3,
 ( #13968, #5083, #18001, #10934 ),
 .UNSPECIFIED., .F., .F.,
 ( 4, 4 ),
 ( 1.514782153580211930E-17, 0.003005512676784846161 ),
 .UNSPECIFIED. ) ;
#8202 = ORIENTED_EDGE ( 'NONE', *, *, #13309, .T. ) ;
#8203 = ORIENTED_EDGE ( 'NONE', *, *, #14495, .T. ) ;
#8204 = CARTESIAN_POINT ( 'NONE',  ( 2.636624412714236865, 15.91454522070173638, 2.161493821596668585 ) ) ;
#8205 = B_SPLINE_CURVE_WITH_KNOTS ( 'NONE', 3,
 ( #5260, #16831, #16925, #3736, #4986, #15486, #9563, #7774, #9286, #15394, #3832, #6714, #4015 ),
 .UNSPECIFIED., .F., .F.,
 ( 4, 3, 3, 3, 4 ),
 ( 3.127317220692750759E-18, 0.0002299804304191474438, 0.0004599608082120254971, 0.0006467586077648028843, 0.0008336169836825993744 ),
 .UNSPECIFIED. ) ;
#8206 = LINE ( 'NONE', #14027, #12664 ) ;
#8207 = CARTESIAN_POINT ( 'NONE',  ( 3.512766787570810845, 10.40533104696146083, -10.87507422923874856 ) ) ;
#8208 = DIRECTION ( 'NONE',  ( 1.000000000000000000, 0.000000000000000000, 0.000000000000000000 ) ) ;
#8209 = CARTESIAN_POINT ( 'NONE',  ( 1.342453679581834924, 9.456403821038797730, 11.38190519890856933 ) ) ;
#8210 = ORIENTED_EDGE ( 'NONE', *, *, #14686, .F. ) ;
#8211 = CARTESIAN_POINT ( 'NONE',  ( 1.846822687350021974, 9.891732594446578375, 7.547953575784160485 ) ) ;
#8212 = EDGE_CURVE ( 'NONE', #14986, #3893, #8504, .T. ) ;
#8213 = EDGE_CURVE ( 'NONE', #5002, #11053, #12368, .T. ) ;
#8214 = CARTESIAN_POINT ( 'NONE',  ( 1.846822687350021974, -11.74004266906801774, -4.121816957446323038 ) ) ;
#8215 = EDGE_CURVE ( 'NONE', #1807, #6378, #1065, .T. ) ;
#8216 = CARTESIAN_POINT ( 'NONE',  ( -6.279379834064045873, 3.098285787164263283, -12.00000000061316108 ) ) ;
#8217 = CARTESIAN_POINT ( 'NONE',  ( 0.3137051932979792457, 13.73004976592202198, 0.4596302728640249136 ) ) ;
#8218 = CIRCLE ( 'NONE', #3931, 10.00000000000000888 ) ;
#8219 = CARTESIAN_POINT ( 'NONE',  ( -26.00000000000001066, -12.50000000000000178, -0.5000000000000000000 ) ) ;
#8220 = CARTESIAN_POINT ( 'NONE',  ( 2.353870697619111496, -0.7635393531607235218, 12.92712089195302561 ) ) ;
#8221 = CYLINDRICAL_SURFACE ( 'NONE', #14076, 5.000000000000000888 ) ;
#8222 = B_SPLINE_CURVE_WITH_KNOTS ( 'NONE', 3,
 ( #7896, #15232, #328, #13505, #6157, #13411, #13315, #9305, #3170, #12269, #10744, #4822, #13706 ),
 .UNSPECIFIED., .F., .F.,
 ( 4, 3, 3, 3, 4 ),
 ( 8.673617379884034509E-19, 0.0002299780670421053329, 0.0004599561239687884940, 0.0006896788984287899067, 0.0009194956271626421231 ),
 .UNSPECIFIED. ) ;
#8223 = CARTESIAN_POINT ( 'NONE',  ( -205.0000000000000000, 4.999999999999974243, 6.000000000000005329 ) ) ;
#8224 = ORIENTED_EDGE ( 'NONE', *, *, #15343, .T. ) ;
#8226 = VERTEX_POINT ( 'NONE', #6016 ) ;
#8225 = CARTESIAN_POINT ( 'NONE',  ( 16.58200780006414732, -0.01115192838421470017, 0.0006320991582340292937 ) ) ;
#8227 = CARTESIAN_POINT ( 'NONE',  ( 3.950837973638675393, -10.51028938476224894, 10.05648675950122595 ) ) ;
#8228 = LINE ( 'NONE', #17015, #9228 ) ;
#8229 = COLOUR_RGB ( '', 0.40784314, 0.44705882, 0.49803922) ;
#8230 = ORIENTED_EDGE ( 'NONE', *, *, #2079, .F. ) ;
#8231 = CARTESIAN_POINT ( 'NONE',  ( 1.847034903785823134, -3.625649561595226888, -11.90269060117937627 ) ) ;
#8232 = B_SPLINE_CURVE_WITH_KNOTS ( 'NONE', 3,
 ( #13802, #4837, #16684, #6456 ),
 .UNSPECIFIED., .F., .F.,
 ( 4, 4 ),
 ( 0.000000000000000000, 0.002004993803842881200 ),
 .UNSPECIFIED. ) ;
#8233 = DIRECTION ( 'NONE',  ( 0.000000000000000000, 8.881784197001252323E-16, 1.000000000000000000 ) ) ;
#8234 = EDGE_LOOP ( 'NONE', ( #1314, #2789, #15805, #17945 ) ) ;
#8235 = CARTESIAN_POINT ( 'NONE',  ( 3.353306896162453477, 9.252610477110421172, -10.44017738170046528 ) ) ;
#8236 = STYLED_ITEM ( 'NONE', ( #4920 ), #3553 ) ;
#8237 = LINE ( 'NONE', #14056, #11284 ) ;
#8238 = CARTESIAN_POINT ( 'NONE',  ( 1.959283090834841090, -12.12982544407802799, -3.239245055717093091 ) ) ;
#8239 = CARTESIAN_POINT ( 'NONE',  ( 0.3145734862173260038, -12.96846406299303212, -4.535879238195068552 ) ) ;
#8240 = CARTESIAN_POINT ( 'NONE',  ( 0.3150690434770172521, -0.1531837610934980720, 13.73846430619029491 ) ) ;
#8241 = ADVANCED_FACE ( 'NONE', ( #8593, #92 ), #17685, .T. ) ;
#8242 = AXIS2_PLACEMENT_3D ( 'NONE', #6705, #17017, #16739 ) ;
#8243 = FILL_AREA_STYLE_COLOUR ( '', #13014 ) ;
#8244 = DIRECTION ( 'NONE',  ( 0.000000000000000000, -1.000000000000000000, 0.000000000000000000 ) ) ;
#8245 = B_SPLINE_CURVE_WITH_KNOTS ( 'NONE', 3,
 ( #7496, #6153, #17622, #9117, #11981, #15984 ),
 .UNSPECIFIED., .F., .F.,
 ( 4, 2, 4 ),
 ( 2.017461075144244397E-18, 0.0002017457492448097769, 0.0004034914984896175480 ),
 .UNSPECIFIED. ) ;
#8246 = CARTESIAN_POINT ( 'NONE',  ( 2.002547531651519996, 9.778737580845815458, -7.942910686618064986 ) ) ;
#8248 = ORIENTED_EDGE ( 'NONE', *, *, #13337, .T. ) ;
#8247 = DIRECTION ( 'NONE',  ( -1.000000000000000000, -0.000000000000000000, -0.000000000000000000 ) ) ;
#8249 = LINE ( 'NONE', #3935, #7879 ) ;
#8250 = ADVANCED_FACE ( 'NONE', ( #4492 ), #15876, .F. ) ;
#8251 = CARTESIAN_POINT ( 'NONE',  ( 0.3142014840576500267, -10.88517824918537080, -8.382000553815572630 ) ) ;
#8252 = CARTESIAN_POINT ( 'NONE',  ( 0.3151930723728477157, -4.172946285306481151, -13.09040889075574476 ) ) ;
#8253 = EDGE_LOOP ( 'NONE', ( #15771, #1475 ) ) ;
#8254 = ORIENTED_EDGE ( 'NONE', *, *, #10930, .T. ) ;
#8255 = CARTESIAN_POINT ( 'NONE',  ( 2.949999999999999734, 0.000000000000000000, 0.000000000000000000 ) ) ;
#8256 = DIRECTION ( 'NONE',  ( -0.000000000000000000, -0.000000000000000000, 1.000000000000000000 ) ) ;
#8257 = ORIENTED_EDGE ( 'NONE', *, *, #2332, .F. ) ;
#8258 = CARTESIAN_POINT ( 'NONE',  ( 1.846138399168762101, -0.4167076046094680408, -12.43476674860266940 ) ) ;
#8259 = PRODUCT_RELATED_PRODUCT_CATEGORY ( 'part', '', ( #206 ) ) ;
#8260 = ADVANCED_FACE ( 'NONE', ( #17383 ), #4297, .T. ) ;
#8261 = DIRECTION ( 'NONE',  ( 0.000000000000000000, 1.000000000000000000, 0.000000000000000000 ) ) ;
#8262 = CARTESIAN_POINT ( 'NONE',  ( -27.50000000000000711, -12.50000000000000178, 3.000000000000000000 ) ) ;
#8263 = EDGE_CURVE ( 'NONE', #8687, #9475, #10122, .T. ) ;
#8264 = EDGE_CURVE ( 'NONE', #12585, #11870, #9612, .T. ) ;
#8265 =( LENGTH_UNIT ( ) NAMED_UNIT ( * ) SI_UNIT ( .MILLI., .METRE. ) );
#8266 = PRODUCT_CONTEXT ( 'NONE', #16819, 'mechanical' ) ;
#8267 = CARTESIAN_POINT ( 'NONE',  ( 0.3720661004400037664, 0.7231997263366731765, -13.79610186261028559 ) ) ;
#8268 = CARTESIAN_POINT ( 'NONE',  ( 0.3145734862173208413, -13.15783074029281963, 3.953068532979947314 ) ) ;
#8269 = CARTESIAN_POINT ( 'NONE',  ( 1.847372867223029846, -3.744745203533896394, -11.86627781945711924 ) ) ;
#8270 = CARTESIAN_POINT ( 'NONE',  ( 16.56753206892534891, -0.006669401563385243120, -0.006760771273035091553 ) ) ;
#8271 = CARTESIAN_POINT ( 'NONE',  ( 1.560000000000000053, 0.000000000000000000, 0.000000000000000000 ) ) ;
#8272 = FACE_OUTER_BOUND ( 'NONE', #18568, .T. ) ;
#8273 = ORIENTED_EDGE ( 'NONE', *, *, #16139, .F. ) ;
#8274 = EDGE_CURVE ( 'NONE', #15252, #14131, #10994, .T. ) ;
#8275 = ORIENTED_EDGE ( 'NONE', *, *, #3603, .T. ) ;
#8276 = ORIENTED_EDGE ( 'NONE', *, *, #1004, .T. ) ;
#8277 = EDGE_LOOP ( 'NONE', ( #6276, #3929, #2225, #11118, #10414, #1704 ) ) ;
#8278 = CARTESIAN_POINT ( 'NONE',  ( 0.4384471787762840855, 12.93784327393180433, -4.978024343488911541 ) ) ;
#8279 = SPHERICAL_SURFACE ( 'NONE', #15407, 5.000000000000000000 ) ;
#8280 = CARTESIAN_POINT ( 'NONE',  ( 2.353870697619111940, 6.980654702310842730, 10.90705766126222187 ) ) ;
#8281 = CARTESIAN_POINT ( 'NONE',  ( 1.342453679581834924, 7.902645620902447376, 12.51077660954468662 ) ) ;
#8282 =( NAMED_UNIT ( * ) PLANE_ANGLE_UNIT ( ) SI_UNIT ( $, .RADIAN. ) );
#8283 = CARTESIAN_POINT ( 'NONE',  ( 0.4384471787762828088, -12.93784327393176881, 4.978024343488995918 ) ) ;
#8284 = AXIS2_PLACEMENT_3D ( 'NONE', #12691, #18521, #11275 ) ;
#8285 = CARTESIAN_POINT ( 'NONE',  ( -30.00000000000000355, -12.50000000000000178, 6.500000000000000888 ) ) ;
#8286 = CARTESIAN_POINT ( 'NONE',  ( 18.75000000000000000, 0.000000000000000000, 2.055000000000000160 ) ) ;
#8287 = DIRECTION ( 'NONE',  ( 0.7635533937278216055, -0.3620487483322484823, -0.5347026451755951815 ) ) ;
#8288 = ORIENTED_EDGE ( 'NONE', *, *, #15650, .T. ) ;
#8289 = VERTEX_POINT ( 'NONE', #9258 ) ;
#8290 = ADVANCED_FACE ( 'NONE', ( #8972 ), #7560, .T. ) ;
#8291 = ORIENTED_EDGE ( 'NONE', *, *, #10957, .F. ) ;
#8292 = ORIENTED_EDGE ( 'NONE', *, *, #14437, .F. ) ;
#8293 = B_SPLINE_CURVE_WITH_KNOTS ( 'NONE', 3,
 ( #13897, #18115, #5015, #16592, #13719, #15244 ),
 .UNSPECIFIED., .F., .F.,
 ( 4, 2, 4 ),
 ( 8.673617379884035472E-19, 0.001500839035891551789, 0.003001678071783102711 ),
 .UNSPECIFIED. ) ;
#8294 = DIRECTION ( 'NONE',  ( 0.000000000000000000, 0.000000000000000000, 1.000000000000000000 ) ) ;
#8295 = CARTESIAN_POINT ( 'NONE',  ( 16.56872352241294521, -0.01033355228142500762, -0.001442253899401184716 ) ) ;
#8296 = CARTESIAN_POINT ( 'NONE',  ( 0.000000000000000000, 1.732050807568878747, 7.017607234860990640E-28 ) ) ;
#8297 = LINE ( 'NONE', #12408, #16377 ) ;
#8298 = CARTESIAN_POINT ( 'NONE',  ( 2.320521194581854463, 13.71278319227944920, 7.743190876766304243 ) ) ;
#8299 = ORIENTED_EDGE ( 'NONE', *, *, #7501, .T. ) ;
#8300 = CARTESIAN_POINT ( 'NONE',  ( 16.56872352241294521, 0.01027347319884441834, -0.001821578298044677175 ) ) ;
#8301 = CARTESIAN_POINT ( 'NONE',  ( 3.950837973638676281, 2.591948120962007884, -14.31366178983250670 ) ) ;
#8302 = CARTESIAN_POINT ( 'NONE',  ( 4.449459268825830982, 7.499999999999999112, -16.63368482084348798 ) ) ;
#8303 = CARTESIAN_POINT ( 'NONE',  ( 1.342453679581834924, -3.649820028552833051, 14.34050741580205823 ) ) ;
#8304 = CIRCLE ( 'NONE', #981, 5.000000000000000888 ) ;
#8305 = CARTESIAN_POINT ( 'NONE',  ( 16.57210152137263393, 0.003862718596009277316, 0.01402404281922923004 ) ) ;
#8306 = CARTESIAN_POINT ( 'NONE',  ( 1.846524061778020531, 3.506196582971103926, 11.93805390544202361 ) ) ;
#8307 = CARTESIAN_POINT ( 'NONE',  ( 0.4384471787762814765, 4.978024343489044767, 12.93784327393174571 ) ) ;
#8308 = CARTESIAN_POINT ( 'NONE',  ( 2.750000000000000000, 0.000000000000000000, 4.750000000000000000 ) ) ;
#8309 = ORIENTED_EDGE ( 'NONE', *, *, #8671, .F. ) ;
#8310 = VERTEX_POINT ( 'NONE', #10509 ) ;
#8311 = B_SPLINE_CURVE_WITH_KNOTS ( 'NONE', 3,
 ( #10258, #10351, #16090, #2974, #7400, #126 ),
 .UNSPECIFIED., .F., .F.,
 ( 4, 2, 4 ),
 ( 3.332294980281255979E-17, 0.0001825746017570583984, 0.0003651492035140835118 ),
 .UNSPECIFIED. ) ;
#8313 = ORIENTED_EDGE ( 'NONE', *, *, #8834, .F. ) ;
#8312 = CARTESIAN_POINT ( 'NONE',  ( 0.3137051932979792457, 12.91601973349270871, 4.679953077377533965 ) ) ;
#8314 = EDGE_CURVE ( 'NONE', #5315, #306, #12040, .T. ) ;
#8315 = EDGE_CURVE ( 'NONE', #8587, #4376, #15775, .T. ) ;
#8316 = EDGE_CURVE ( 'NONE', #7381, #14945, #8050, .T. ) ;
#8317 = AXIS2_PLACEMENT_3D ( 'NONE', #10456, #7505, #6160 ) ;
#8318 = CARTESIAN_POINT ( 'NONE',  ( 11.50000000000000178, 0.000000000000000000, 10.50000000000000000 ) ) ;
#8319 = VERTEX_POINT ( 'NONE', #6203 ) ;
#8320 = CARTESIAN_POINT ( 'NONE',  ( 2.705023505549863039, 13.27418276223636084, -0.8488853074253436271 ) ) ;
#8321 = B_SPLINE_CURVE_WITH_KNOTS ( 'NONE', 3,
 ( #3709, #18243, #16989, #6401, #663, #10797 ),
 .UNSPECIFIED., .F., .F.,
 ( 4, 2, 4 ),
 ( 8.673617379884035472E-19, 0.001500839035891552223, 0.003001678071783103578 ),
 .UNSPECIFIED. ) ;
#8322 = DIRECTION ( 'NONE',  ( -1.000000000000000000, -0.000000000000000000, -0.000000000000000000 ) ) ;
#8323 = DIRECTION ( 'NONE',  ( -1.000000000000000000, -0.000000000000000000, 0.000000000000000000 ) ) ;
#8324 = VERTEX_POINT ( 'NONE', #4873 ) ;
#8325 = CARTESIAN_POINT ( 'NONE',  ( 2.002547531651519996, 7.942910686618313676, -9.778737580845612953 ) ) ;
#8326 = CARTESIAN_POINT ( 'NONE',  ( 2.002547531651519996, 7.942910686618313676, -9.778737580845612953 ) ) ;
#8327 = DIRECTION ( 'NONE',  ( -1.000000000000000000, -0.000000000000000000, -0.000000000000000000 ) ) ;
#8328 = CARTESIAN_POINT ( 'NONE',  ( 0.3145729642390373559, -13.15786090015081555, -3.952965287571249764 ) ) ;
#8329 = EDGE_CURVE ( 'NONE', #10646, #9529, #476, .T. ) ;
#8330 = DIRECTION ( 'NONE',  ( 0.000000000000000000, 0.000000000000000000, 1.000000000000000000 ) ) ;
#8331 = B_SPLINE_CURVE_WITH_KNOTS ( 'NONE', 3,
 ( #9318, #15147, #432, #7905, #16401, #4732 ),
 .UNSPECIFIED., .F., .F.,
 ( 4, 2, 4 ),
 ( 4.016409351050315258E-17, 0.0002014099069817277545, 0.0004028198139634153394 ),
 .UNSPECIFIED. ) ;
#8332 = SURFACE_STYLE_FILL_AREA ( #1050 ) ;
#8333 = CARTESIAN_POINT ( 'NONE',  ( 1.254009781012255020, 7.789615163754674221, -12.44229282923133262 ) ) ;
#8334 = CARTESIAN_POINT ( 'NONE',  ( -58.82978549640777288, -10.68512861272757952, 3.000000000000000000 ) ) ;
#8336 = EDGE_LOOP ( 'NONE', ( #6248, #9207, #7434, #12132 ) ) ;
#8335 = DIRECTION ( 'NONE',  ( -1.000000000000000000, 0.000000000000000000, 0.000000000000000000 ) ) ;
#8337 = FACE_BOUND ( 'NONE', #10112, .T. ) ;
#8338 = CARTESIAN_POINT ( 'NONE',  ( 1.560000000000000053, -0.8660254037844384856, -1.500000000000000000 ) ) ;
#8339 = CARTESIAN_POINT ( 'NONE',  ( 0.3150692679895970572, -4.099798979280757649, -13.11337225490256664 ) ) ;
#8340 = ORIENTED_EDGE ( 'NONE', *, *, #14863, .T. ) ;
#8341 = CARTESIAN_POINT ( 'NONE',  ( -4.000000000000000000, 20.00000000000000000, 8.000000000000000000 ) ) ;
#8342 = ADVANCED_FACE ( 'NONE', ( #578, #11943 ), #4963, .F. ) ;
#8343 = CARTESIAN_POINT ( 'NONE',  ( 16.57210152137263393, -0.003862718596009374894, -0.01402404281922920576 ) ) ;
#8344 = VERTEX_POINT ( 'NONE', #1813 ) ;
#8345 = CARTESIAN_POINT ( 'NONE',  ( 0.3137051932979809665, 3.805684345189785933, 13.20008686438107581 ) ) ;
#8346 = CARTESIAN_POINT ( 'NONE',  ( 16.56782317627811096, 0.008141063682853404496, 0.005492611183757338013 ) ) ;
#8347 = CARTESIAN_POINT ( 'NONE',  ( 0.3132642857406501280, 11.41580579227788128, -7.641821025099742926 ) ) ;
#8348 = CARTESIAN_POINT ( 'NONE',  ( 1.846613052777651198, -9.862487290071051405, 7.585914669018136713 ) ) ;
#8349 = EDGE_CURVE ( 'NONE', #17715, #11214, #17874, .T. ) ;
#8350 = VECTOR ( 'NONE', #9292, 1000.000000000000000 ) ;
#8351 = PRODUCT_CONTEXT ( 'NONE', #2754, 'mechanical' ) ;
#8352 =( BOUNDED_SURFACE ( )  B_SPLINE_SURFACE ( 3, 1, ( 
 ( #7522, #17276 ),
 ( #13339, #12878 ),
 ( #15845, #3190 ),
 ( #346, #17646 ) ),
 .UNSPECIFIED., .F., .F., .T. ) 
 B_SPLINE_SURFACE_WITH_KNOTS ( ( 4, 4 ),
 ( 2, 2 ),
 ( 0.000000000000000000, 1.000000000000000000 ),
 ( 0.000000000000000000, 1.000000000000000000 ),
 .UNSPECIFIED. ) 
 GEOMETRIC_REPRESENTATION_ITEM ( )  RATIONAL_B_SPLINE_SURFACE ( (
 ( 1.000000000000000000, 1.000000000000000000),
 ( 0.9593108457356467333, 0.9995965569486454649),
 ( 0.9593108457356467333, 0.9995965569486454649),
 ( 1.000000000000000000, 1.000000000000000000) ) ) 
 REPRESENTATION_ITEM ( '' )  SURFACE ( )  );
#8353 = LINE ( 'NONE', #12826, #8638 ) ;
#8354 = LINE ( 'NONE', #2595, #14273 ) ;
#8355 = CARTESIAN_POINT ( 'NONE',  ( 1.847168016377986000, -4.022276579849877187, -11.77471791462002670 ) ) ;
#8356 = CARTESIAN_POINT ( 'NONE',  ( 0.3095370825347224519, 10.84046130709070788, -8.444334731363888125 ) ) ;
#8357 = LINE ( 'NONE', #14361, #5098 ) ;
#8358 = VERTEX_POINT ( 'NONE', #7656 ) ;
#8359 = CARTESIAN_POINT ( 'NONE',  ( 0.3148213771069364175, 11.24846294176323447, -7.888490156175093304 ) ) ;
#8360 = CARTESIAN_POINT ( 'NONE',  ( 1.861706995891668104, 6.878962591851903063, -10.38589138506418408 ) ) ;
#8361 = VERTEX_POINT ( 'NONE', #4586 ) ;
#8362 = ORIENTED_EDGE ( 'NONE', *, *, #17496, .T. ) ;
#8363 = AXIS2_PLACEMENT_3D ( 'NONE', #14904, #7848, #10802 ) ;
#8364 = ORIENTED_EDGE ( 'NONE', *, *, #8735, .F. ) ;
#8365 = EDGE_LOOP ( 'NONE', ( #3894, #17351, #2001, #17258 ) ) ;
#8366 = CARTESIAN_POINT ( 'NONE',  ( -6.538348415311006967, 2.499999999999998668, -17.00000000000000000 ) ) ;
#8367 = ADVANCED_FACE ( 'NONE', ( #12141 ), #13462, .F. ) ;
#8368 = ADVANCED_FACE ( 'NONE', ( #14802 ), #17270, .F. ) ;
#8369 = FILL_AREA_STYLE_COLOUR ( '', #1396 ) ;
#8370 = CARTESIAN_POINT ( 'NONE',  ( 0.3307726912345239634, -12.88561780039862015, 4.812300915532924606 ) ) ;
#8371 = CIRCLE ( 'NONE', #13865, 2.500000000000000000 ) ;
#8372 = LINE ( 'NONE', #13331, #5889 ) ;
#8373 = VERTEX_POINT ( 'NONE', #10798 ) ;
#8374 = ORIENTED_EDGE ( 'NONE', *, *, #10047, .F. ) ;
#8375 = EDGE_LOOP ( 'NONE', ( #16741, #10834, #997, #3319 ) ) ;
#8376 =( BOUNDED_SURFACE ( )  B_SPLINE_SURFACE ( 3, 1, ( 
 ( #7508, #17827 ),
 ( #3376, #1865 ),
 ( #15144, #13511 ),
 ( #17732, #16195 ) ),
 .UNSPECIFIED., .F., .F., .T. ) 
 B_SPLINE_SURFACE_WITH_KNOTS ( ( 4, 4 ),
 ( 2, 2 ),
 ( 0.000000000000000000, 1.000000000000000000 ),
 ( 0.000000000000000000, 1.000000000000000000 ),
 .UNSPECIFIED. ) 
 GEOMETRIC_REPRESENTATION_ITEM ( )  RATIONAL_B_SPLINE_SURFACE ( (
 ( 1.000000000000000000, 1.000000000000000000),
 ( 0.9933953342250438912, 0.8357391271907739227),
 ( 0.9933953342250438912, 0.8357391271907739227),
 ( 1.000000000000000000, 1.000000000000000000) ) ) 
 REPRESENTATION_ITEM ( '' )  SURFACE ( )  );
#8377 = VERTEX_POINT ( 'NONE', #665 ) ;
#8378 =( BOUNDED_SURFACE ( )  B_SPLINE_SURFACE ( 3, 1, ( 
 ( #13837, #2446 ),
 ( #8026, #3897 ),
 ( #10987, #14028 ),
 ( #12406, #2104 ) ),
 .UNSPECIFIED., .F., .F., .T. ) 
 B_SPLINE_SURFACE_WITH_KNOTS ( ( 4, 4 ),
 ( 2, 2 ),
 ( 0.000000000000000000, 1.000000000000000000 ),
 ( 0.000000000000000000, 1.000000000000000000 ),
 .UNSPECIFIED. ) 
 GEOMETRIC_REPRESENTATION_ITEM ( )  RATIONAL_B_SPLINE_SURFACE ( (
 ( 1.000000000000000000, 1.000000000000000000),
 ( 0.7792777138730160313, 0.9689936506012927220),
 ( 0.7792777138730160313, 0.9689936506012927220),
 ( 1.000000000000000000, 1.000000000000000000) ) ) 
 REPRESENTATION_ITEM ( '' )  SURFACE ( )  );
#8379 = CIRCLE ( 'NONE', #11213, 7.000000000000000000 ) ;
#8380 = CARTESIAN_POINT ( 'NONE',  ( -30.00000000000000355, -12.50000000000000178, 7.000000000000000000 ) ) ;
#8381 = CARTESIAN_POINT ( 'NONE',  ( 16.56753206892534891, -0.008490833999798956880, -0.004253784598196145433 ) ) ;
#8382 = CARTESIAN_POINT ( 'NONE',  ( 0.4754618798421162973, 13.89949764182682657, 0.7484603771384912285 ) ) ;
#8383 = CARTESIAN_POINT ( 'NONE',  ( 12.00000000000000711, -15.99999999999999645, 8.000000000000000000 ) ) ;
#8384 = SURFACE_STYLE_FILL_AREA ( #16895 ) ;
#8385 = ORIENTED_EDGE ( 'NONE', *, *, #17769, .T. ) ;
#8386 = CARTESIAN_POINT ( 'NONE',  ( 3.950837973638668288, 0.000000000000000000, 0.000000000000000000 ) ) ;
#8387 = EDGE_CURVE ( 'NONE', #9890, #421, #17369, .T. ) ;
#8388 = CARTESIAN_POINT ( 'NONE',  ( 1.959212340397940899, -12.12975361829678178, 3.239239832448982170 ) ) ;
#8389 = CARTESIAN_POINT ( 'NONE',  ( 0.6549932209177148357, 7.499999999999867661, -13.04593603512842570 ) ) ;
#8390 = DIRECTION ( 'NONE',  ( 1.000000000000000000, 0.000000000000000000, 0.000000000000000000 ) ) ;
#8391 = CARTESIAN_POINT ( 'NONE',  ( 1.977228804421385044, 15.04020501276069588, 3.321884655132254505 ) ) ;
#8392 = EDGE_CURVE ( 'NONE', #8961, #8612, #12101, .T. ) ;
#8393 = FACE_BOUND ( 'NONE', #17147, .T. ) ;
#8394 = CARTESIAN_POINT ( 'NONE',  ( -6.538348415311014072, -7.500000000000000888, -16.99999999999999645 ) ) ;
#8395 = CARTESIAN_POINT ( 'NONE',  ( 1.847372867223022963, -3.945260592619128204, 11.80112642014553614 ) ) ;
#8396 = EDGE_LOOP ( 'NONE', ( #10238, #11352, #1165, #3057 ) ) ;
#8397 = CONICAL_SURFACE ( 'NONE', #8115, 2.500000000000000000, 1.029744258676656754 ) ;
#8398 = CONICAL_SURFACE ( 'NONE', #5043, 14.54644660717763927, 0.8559913436420816257 ) ;
#8400 = ORIENTED_EDGE ( 'NONE', *, *, #10518, .T. ) ;
#8399 = CARTESIAN_POINT ( 'NONE',  ( -30.00000000000000355, -12.50000000000000178, 3.000000000000000000 ) ) ;
#8401 = DIRECTION ( 'NONE',  ( -1.000000000000000000, 0.000000000000000000, 0.000000000000000000 ) ) ;
#8402 = VECTOR ( 'NONE', #13270, 1000.000000000000114 ) ;
#8403 = CARTESIAN_POINT ( 'NONE',  ( -30.00000000000000355, -12.50000000000000178, -7.071067811865460406 ) ) ;
#8404 = ORIENTED_EDGE ( 'NONE', *, *, #4097, .F. ) ;
#8405 = DIRECTION ( 'NONE',  ( 0.000000000000000000, 0.000000000000000000, 1.000000000000000000 ) ) ;
#8406 = CARTESIAN_POINT ( 'NONE',  ( -6.234321419756340354, -7.500000000000000888, -16.99999999998787104 ) ) ;
#8407 = CARTESIAN_POINT ( 'NONE',  ( 0.4862570985993235340, 10.79774104611385965, -8.769551628660616771 ) ) ;
#8408 = ORIENTED_EDGE ( 'NONE', *, *, #6121, .T. ) ;
#8409 = LINE ( 'NONE', #14417, #9303 ) ;
#8410 = DIRECTION ( 'NONE',  ( 0.000000000000000000, 0.000000000000000000, 1.000000000000000000 ) ) ;
#8411 = MECHANICAL_DESIGN_GEOMETRIC_PRESENTATION_REPRESENTATION (  '', ( #12079 ), #178 ) ;
#8412 = CARTESIAN_POINT ( 'NONE',  ( 0.3150686449036029235, -13.73846184595214304, 0.1533607327085267646 ) ) ;
#8413 = VECTOR ( 'NONE', #6502, 999.9999999999998863 ) ;
#8414 = CARTESIAN_POINT ( 'NONE',  ( 16.57210152137263393, 0.0006600038696346007027, -0.01453130299868522768 ) ) ;
#8415 = LINE ( 'NONE', #14247, #3185 ) ;
#8416 = EDGE_CURVE ( 'NONE', #885, #3195, #6858, .T. ) ;
#8417 = PLANE ( 'NONE',  #2245 ) ;
#8418 = CARTESIAN_POINT ( 'NONE',  ( 0.3095370825347233956, -10.84046130709064393, 8.444334731363969837 ) ) ;
#8420 = ORIENTED_EDGE ( 'NONE', *, *, #3209, .T. ) ;
#8419 = CARTESIAN_POINT ( 'NONE',  ( 1.342453679581834924, 3.649820028552730022, 14.34050741580208133 ) ) ;
#8421 = CARTESIAN_POINT ( 'NONE',  ( 0.3137051932979792457, 0.4596302728641686874, -13.73004976592201487 ) ) ;
#8422 = CARTESIAN_POINT ( 'NONE',  ( -1.500000000000001332, 6.799999999999999822, 5.000000000000000000 ) ) ;
#8423 = COLOUR_RGB ( '', 0.31764706, 0.68627451, 0.89019608) ;
#8424 = EDGE_LOOP ( 'NONE', ( #17771, #9102, #12652, #16137, #14259, #3295 ) ) ;
#8425 = CARTESIAN_POINT ( 'NONE',  ( 0.3142011359265305392, 3.879426116491875742, -13.17934269988453977 ) ) ;
#8426 = CARTESIAN_POINT ( 'NONE',  ( 1.560000000000000053, -1.732050807568877859, -1.752539433813135784E-17 ) ) ;
#8427 = ORIENTED_EDGE ( 'NONE', *, *, #15219, .T. ) ;
#8428 = CARTESIAN_POINT ( 'NONE',  ( 0.3145734862173267810, 3.953068532979994831, 13.15783074029279831 ) ) ;
#8429 = CARTESIAN_POINT ( 'NONE',  ( 1.846138399168762101, -9.815003036200465658, 7.646096044339859787 ) ) ;
#8430 = B_SPLINE_CURVE_WITH_KNOTS ( 'NONE', 3,
 ( #11401, #2862, #5377, #15881, #13010, #17220, #18844, #4133, #15787, #4036 ),
 .UNSPECIFIED., .F., .F.,
 ( 4, 3, 3, 4 ),
 ( 0.0004597478348665241538, 0.0004599561239687906082, 0.0006896788984287882803, 0.0009194956271626397379 ),
 .UNSPECIFIED. ) ;
#8431 = LINE ( 'NONE', #1354, #12203 ) ;
#8432 = CARTESIAN_POINT ( 'NONE',  ( 0.4862570985993235340, 12.97920246947886191, -5.003653737315353567 ) ) ;
#8433 = CARTESIAN_POINT ( 'NONE',  ( 3.686287386450715076E-15, -16.60000000000000142, 21.01316734529526187 ) ) ;
#8434 = UNCERTAINTY_MEASURE_WITH_UNIT (LENGTH_MEASURE( 1.000000000000000082E-05 ), #2113, 'distance_accuracy_value', 'NONE');
#8435 = EDGE_CURVE ( 'NONE', #3893, #400, #11181, .T. ) ;
#8436 = EDGE_CURVE ( 'NONE', #9382, #3145, #5145, .T. ) ;
#8437 = VERTEX_POINT ( 'NONE', #17082 ) ;
#8438 = EDGE_CURVE ( 'NONE', #7261, #18407, #3544, .T. ) ;
#8439 = CARTESIAN_POINT ( 'NONE',  ( -194.9999999999999716, 4.999999999999973355, -153.7432847437423789 ) ) ;
#8440 = CARTESIAN_POINT ( 'NONE',  ( 1.918921323896325193, -0.6349083173281016013, 12.49850046818174043 ) ) ;
#8441 = LINE ( 'NONE', #1179, #1959 ) ;
#8442 = CARTESIAN_POINT ( 'NONE',  ( 3.950837973638676281, -12.81214529934970336, -6.888253895133431115 ) ) ;
#8443 = DIRECTION ( 'NONE',  ( -0.000000000000000000, -0.000000000000000000, 1.000000000000000000 ) ) ;
#8444 = AXIS2_PLACEMENT_3D ( 'NONE', #2394, #7085, #6804 ) ;
#8445 = ORIENTED_EDGE ( 'NONE', *, *, #12873, .T. ) ;
#8446 = CARTESIAN_POINT ( 'NONE',  ( 2.697797270744666687, -10.19107313879051269, -8.537712152180978009 ) ) ;
#8447 = CARTESIAN_POINT ( 'NONE',  ( 16.56872352241294521, 0.001821578298043785094, -0.01027347319884367241 ) ) ;
#8448 = ORIENTED_EDGE ( 'NONE', *, *, #2407, .T. ) ;
#8449 = CIRCLE ( 'NONE', #18824, 5.000000000000000888 ) ;
#8450 = TOROIDAL_SURFACE ( 'NONE', #7553, 5.000000000000005329, 5.000000000000000000 ) ;
#8451 = EDGE_LOOP ( 'NONE', ( #10961, #11260, #2702, #1269, #10386 ) ) ;
#8452 = ORIENTED_EDGE ( 'NONE', *, *, #4517, .F. ) ;
#8453 = DIRECTION ( 'NONE',  ( -1.000000000000000000, -0.000000000000000000, -0.000000000000000000 ) ) ;
#8454 =( GEOMETRIC_REPRESENTATION_CONTEXT ( 3 ) GLOBAL_UNCERTAINTY_ASSIGNED_CONTEXT ( ( #13228 ) ) GLOBAL_UNIT_ASSIGNED_CONTEXT ( ( #17202, #18446, #9835 ) ) REPRESENTATION_CONTEXT ( 'NONE', 'WORKASPACE' ) );
#8455 = ORIENTED_EDGE ( 'NONE', *, *, #18860, .T. ) ;
#8456 = VECTOR ( 'NONE', #13583, 1000.000000000000000 ) ;
#8457 = B_SPLINE_CURVE_WITH_KNOTS ( 'NONE', 3,
 ( #2893, #16110, #1489, #13139 ),
 .UNSPECIFIED., .F., .F.,
 ( 4, 4 ),
 ( 2.006682199098010609E-17, 0.003005512676784846595 ),
 .UNSPECIFIED. ) ;
#8458 = DIRECTION ( 'NONE',  ( 0.000000000000000000, 0.000000000000000000, 1.000000000000000000 ) ) ;
#8459 =( BOUNDED_SURFACE ( )  B_SPLINE_SURFACE ( 3, 1, ( 
 ( #11385, #16838 ),
 ( #11111, #11298 ),
 ( #2479, #8152 ),
 ( #6718, #12718 ) ),
 .UNSPECIFIED., .F., .F., .T. ) 
 B_SPLINE_SURFACE_WITH_KNOTS ( ( 4, 4 ),
 ( 2, 2 ),
 ( 0.000000000000000000, 1.000000000000000000 ),
 ( 0.000000000000000000, 1.000000000000000000 ),
 .UNSPECIFIED. ) 
 GEOMETRIC_REPRESENTATION_ITEM ( )  RATIONAL_B_SPLINE_SURFACE ( (
 ( 1.000000000000000000, 1.000000000000000000),
 ( 0.9593108457356467333, 0.9995965569486454649),
 ( 0.9593108457356467333, 0.9995965569486454649),
 ( 1.000000000000000000, 1.000000000000000000) ) ) 
 REPRESENTATION_ITEM ( '' )  SURFACE ( )  );
#8460 = CARTESIAN_POINT ( 'NONE',  ( 0.000000000000000000, 0.000000000000000000, 0.000000000000000000 ) ) ;
#8461 = DIRECTION ( 'NONE',  ( 0.000000000000000000, 1.000000000000000000, 0.000000000000000000 ) ) ;
#8462 = LINE ( 'NONE', #17063, #7512 ) ;
#8463 = CIRCLE ( 'NONE', #16717, 5.000000000000049738 ) ;
#8464 = CARTESIAN_POINT ( 'NONE',  ( -19.99999999999999645, 7.499999999999999112, -17.00000000000000000 ) ) ;
#8465 = PLANE ( 'NONE',  #10151 ) ;
#8466 = DIRECTION ( 'NONE',  ( -1.540743955509788340E-33, -1.000000000000000000, -2.533398541561209262E-17 ) ) ;
#8467 = ADVANCED_FACE ( 'NONE', ( #5048 ), #6684, .T. ) ;
#8468 = CARTESIAN_POINT ( 'NONE',  ( 16.57778382496167424, -0.01306626476309294925, 0.007244066302946726259 ) ) ;
#8469 = CARTESIAN_POINT ( 'NONE',  ( 0.4754618798421171855, 5.007009103465246191, 12.98792082933646519 ) ) ;
#8470 = VERTEX_POINT ( 'NONE', #16806 ) ;
#8471 = B_SPLINE_CURVE_WITH_KNOTS ( 'NONE', 3,
 ( #4077, #17165, #14307, #14212, #17080, #15630 ),
 .UNSPECIFIED., .F., .F.,
 ( 4, 2, 4 ),
 ( 0.000000000000000000, 0.001500839035891552223, 0.003001678071783104446 ),
 .UNSPECIFIED. ) ;
#8472 = ORIENTED_EDGE ( 'NONE', *, *, #18239, .F. ) ;
#8473 = AXIS2_PLACEMENT_3D ( 'NONE', #8285, #18494, #17250 ) ;
#8474 = ORIENTED_EDGE ( 'NONE', *, *, #8544, .F. ) ;
#8475 = ORIENTED_EDGE ( 'NONE', *, *, #11297, .T. ) ;
#8476 = B_SPLINE_CURVE_WITH_KNOTS ( 'NONE', 3,
 ( #6595, #5150, #15373, #6316 ),
 .UNSPECIFIED., .F., .F.,
 ( 4, 4 ),
 ( 1.974081779422029518E-17, 0.003005512676784849631 ),
 .UNSPECIFIED. ) ;
#8477 = DIRECTION ( 'NONE',  ( 0.4246593920385850485, 0.1376957914266804250, -0.8948208031649687033 ) ) ;
#8478 = FACE_OUTER_BOUND ( 'NONE', #18150, .T. ) ;
#8479 = CARTESIAN_POINT ( 'NONE',  ( 0.3151928476913555821, 8.075547435847115096, -11.11539186930577827 ) ) ;
#8480 = ORIENTED_EDGE ( 'NONE', *, *, #10490, .F. ) ;
#8481 = CARTESIAN_POINT ( 'NONE',  ( -194.9999999999999716, -30.00000000000003197, 3.000000000000000000 ) ) ;
#8482 = CARTESIAN_POINT ( 'NONE',  ( 0.3307726912345187453, 0.5948952607472642873, 13.74203354050372461 ) ) ;
#8483 = CARTESIAN_POINT ( 'NONE',  ( 2.817269318715503790, 7.499999999999999112, -15.81922481682711634 ) ) ;
#8484 = CARTESIAN_POINT ( 'NONE',  ( 0.8740779401510758717, -0.8420120399581221271, -14.27348745891595172 ) ) ;
#8485 = EDGE_CURVE ( 'NONE', #8069, #12401, #1716, .T. ) ;
#8486 = ADVANCED_FACE ( 'NONE', ( #12583, #6588 ), #2273, .T. ) ;
#8487 = VECTOR ( 'NONE', #858, 1000.000000000000000 ) ;
#8488 = CARTESIAN_POINT ( 'NONE',  ( 3.950837973638676281, -12.81214529934979929, 6.888253895133251703 ) ) ;
#8489 = DIRECTION ( 'NONE',  ( -0.7561779333270775005, -0.5491072561318312006, -0.3559159372837374935 ) ) ;
#8490 = EDGE_CURVE ( 'NONE', #9334, #369, #8297, .T. ) ;
#8491 = FACE_OUTER_BOUND ( 'NONE', #17022, .T. ) ;
#8492 = CARTESIAN_POINT ( 'NONE',  ( 0.4862570985993235340, -5.003653737315397976, -12.97920246947884770 ) ) ;
#8493 = ORIENTED_EDGE ( 'NONE', *, *, #15182, .T. ) ;
#8494 = VECTOR ( 'NONE', #12537, 1000.000000000000114 ) ;
#8496 = ORIENTED_EDGE ( 'NONE', *, *, #7743, .T. ) ;
#8495 = FACE_OUTER_BOUND ( 'NONE', #2077, .T. ) ;
#8497 = CARTESIAN_POINT ( 'NONE',  ( 3.950837973638675393, 6.888253895133479965, -12.81214529934967672 ) ) ;
#8498 = DIRECTION ( 'NONE',  ( 0.000000000000000000, 0.000000000000000000, 1.000000000000000000 ) ) ;
#8499 = EDGE_CURVE ( 'NONE', #5275, #3136, #1111, .T. ) ;
#8500 = VERTEX_POINT ( 'NONE', #10900 ) ;
#8501 = CARTESIAN_POINT ( 'NONE',  ( -1.979226605763932723, -14.99999999999999645, 6.000000000000000000 ) ) ;
#8502 = CARTESIAN_POINT ( 'NONE',  ( 1.562796894703937678, 0.000000000000000000, 0.000000000000000000 ) ) ;
#8503 = CARTESIAN_POINT ( 'NONE',  ( 0.4754618798421162973, 7.564402563418637371, -11.68486377711958468 ) ) ;
#8504 = LINE ( 'NONE', #13080, #15123 ) ;
#8505 = ORIENTED_EDGE ( 'NONE', *, *, #8895, .F. ) ;
#8506 = DIRECTION ( 'NONE',  ( -1.000000000000000000, -5.782411586589358625E-16, 0.000000000000000000 ) ) ;
#8507 = EDGE_CURVE ( 'NONE', #617, #10695, #6962, .T. ) ;
#8508 = CARTESIAN_POINT ( 'NONE',  ( 1.562796894703937678, 1.488975241814732168E-15, 12.15840553252917289 ) ) ;
#8509 = CARTESIAN_POINT ( 'NONE',  ( 3.512766787570762439, -10.40533104696141997, 10.87507422923886224 ) ) ;
#8510 = LINE ( 'NONE', #5530, #3535 ) ;
#8511 = DIRECTION ( 'NONE',  ( -1.000000000000000000, 0.000000000000000000, 0.000000000000000000 ) ) ;
#8512 = B_SPLINE_CURVE_WITH_KNOTS ( 'NONE', 3,
 ( #1693, #11730, #17560, #10298 ),
 .UNSPECIFIED., .F., .F.,
 ( 4, 4 ),
 ( 1.684670163748776910E-17, 0.003005512676784852233 ),
 .UNSPECIFIED. ) ;
#8513 = CARTESIAN_POINT ( 'NONE',  ( 2.426025403784448642, 2.655529440325959183E-32, -2.168404344971008868E-16 ) ) ;
#8514 = VECTOR ( 'NONE', #6912, 999.9999999999998863 ) ;
#8515 = DIRECTION ( 'NONE',  ( -1.000000000000000000, 0.000000000000000000, 0.000000000000000000 ) ) ;
#8517 = ORIENTED_EDGE ( 'NONE', *, *, #16832, .F. ) ;
#8516 = CARTESIAN_POINT ( 'NONE',  ( 1.104287921197080512E-14, -9.013167318348349610, 25.01316734529528674 ) ) ;
#8518 = CARTESIAN_POINT ( 'NONE',  ( 3.353306896162455697, -5.573563251762193360, 12.78841260990236428 ) ) ;
#8519 = FACE_OUTER_BOUND ( 'NONE', #17814, .T. ) ;
#8520 = ADVANCED_FACE ( 'NONE', ( #5325 ), #15763, .F. ) ;
#8521 = EDGE_LOOP ( 'NONE', ( #6243, #17096, #6694, #13724 ) ) ;
#8522 = DIRECTION ( 'NONE',  ( -0.7561779333270775005, 0.1688126975276644792, -0.6322161072786924851 ) ) ;
#8523 = FACE_OUTER_BOUND ( 'NONE', #14812, .T. ) ;
#8524 = VERTEX_POINT ( 'NONE', #15363 ) ;
#8525 = FACE_OUTER_BOUND ( 'NONE', #12309, .T. ) ;
#8526 = FILL_AREA_STYLE ('',( #9952 ) ) ;
#8527 = CARTESIAN_POINT ( 'NONE',  ( 0.4862570985993252548, 3.580942890621670482, 13.44146924561382583 ) ) ;
#8528 = CIRCLE ( 'NONE', #2713, 5.000000000000000888 ) ;
#8529 = CARTESIAN_POINT ( 'NONE',  ( 2.636624412714236865, 0.000000000000000000, 0.000000000000000000 ) ) ;
#8531 = CARTESIAN_POINT ( 'NONE',  ( 1.846138399168762989, 11.95493567637850774, 3.446241763653039580 ) ) ;
#8530 = VECTOR ( 'NONE', #12709, 1000.000000000000000 ) ;
#8532 = ORIENTED_EDGE ( 'NONE', *, *, #16501, .F. ) ;
#8533 = CONTEXT_DEPENDENT_SHAPE_REPRESENTATION ( #13038, #13656 ) ;
#8534 = DIRECTION ( 'NONE',  ( -0.000000000000000000, 0.000000000000000000, 1.000000000000000000 ) ) ;
#8535 = CARTESIAN_POINT ( 'NONE',  ( 2.002547531651519996, -0.6781519942172617998, 12.57989064830759318 ) ) ;
#8536 = CARTESIAN_POINT ( 'NONE',  ( 1.847168016377985778, 0.1868244120189564983, 12.44137401948661115 ) ) ;
#8537 = CARTESIAN_POINT ( 'NONE',  ( 16.57210152137263393, -0.01136813053532154116, 0.009075239946109162070 ) ) ;
#8538 = LINE ( 'NONE', #12831, #18225 ) ;
#8539 = ORIENTED_EDGE ( 'NONE', *, *, #2491, .F. ) ;
#8540 = CARTESIAN_POINT ( 'NONE',  ( 1.254009781011695468, -14.24044713813331597, -3.563484327698402510 ) ) ;
#8541 = EDGE_LOOP ( 'NONE', ( #165, #5558, #11197, #6658 ) ) ;
#8542 = ADVANCED_FACE ( 'NONE', ( #2447 ), #11265, .T. ) ;
#8543 = EDGE_CURVE ( 'NONE', #5397, #14601, #250, .T. ) ;
#8544 = EDGE_CURVE ( 'NONE', #15569, #5801, #8140, .T. ) ;
#8545 = ORIENTED_EDGE ( 'NONE', *, *, #1307, .T. ) ;
#8546 = CARTESIAN_POINT ( 'NONE',  ( 16.56679352167444819, 0.004162264567718796174, -0.008311568981097996328 ) ) ;
#8547 = ORIENTED_EDGE ( 'NONE', *, *, #17014, .F. ) ;
#8548 = ORIENTED_EDGE ( 'NONE', *, *, #8059, .F. ) ;
#8549 = B_SPLINE_CURVE_WITH_KNOTS ( 'NONE', 3,
 ( #9144, #8761, #13149, #60, #11720, #1885 ),
 .UNSPECIFIED., .F., .F.,
 ( 4, 2, 4 ),
 ( 8.673617379884035472E-19, 0.0001828790815886942919, 0.0003657581631773877164 ),
 .UNSPECIFIED. ) ;
#8550 = CARTESIAN_POINT ( 'NONE',  ( 1.977228804421386821, 10.21522664410325021, 11.52787183731143017 ) ) ;
#8551 = CARTESIAN_POINT ( 'NONE',  ( 0.3145729642390390768, 12.96842777670212676, -4.535980493004950986 ) ) ;
#8552 = CARTESIAN_POINT ( 'NONE',  ( 16.56782317627811096, 0.002708056627498641941, 0.009439921864426896805 ) ) ;
#8553 = DIRECTION ( 'NONE',  ( 0.000000000000000000, 0.000000000000000000, 1.000000000000000000 ) ) ;
#8554 = CARTESIAN_POINT ( 'NONE',  ( 0.000000000000000000, 0.000000000000000000, 0.000000000000000000 ) ) ;
#8555 = CARTESIAN_POINT ( 'NONE',  ( 0.3137051932979792457, -13.73004976592202375, 0.4596302728639276580 ) ) ;
#8556 = CARTESIAN_POINT ( 'NONE',  ( 16.57778382496167424, -0.01466529584256786797, -0.002851818597093949692 ) ) ;
#8557 = CARTESIAN_POINT ( 'NONE',  ( 0.3148213771069329203, -13.13560149728604109, 4.026433757158931925 ) ) ;
#8558 = CARTESIAN_POINT ( 'NONE',  ( 1.342453679581834924, 5.476372339890016150, 13.74702459364886487 ) ) ;
#8559 = VERTEX_POINT ( 'NONE', #9997 ) ;
#8560 = ORIENTED_EDGE ( 'NONE', *, *, #7208, .T. ) ;
#8561 = EDGE_LOOP ( 'NONE', ( #14363, #10166, #17766, #13829 ) ) ;
#8562 = ORIENTED_EDGE ( 'NONE', *, *, #15010, .T. ) ;
#8563 = VERTEX_POINT ( 'NONE', #4274 ) ;
#8564 =( BOUNDED_SURFACE ( )  B_SPLINE_SURFACE ( 3, 1, ( 
 ( #9996, #17356 ),
 ( #18788, #15829 ),
 ( #11822, #16014 ),
 ( #16216, #11627 ) ),
 .UNSPECIFIED., .F., .F., .T. ) 
 B_SPLINE_SURFACE_WITH_KNOTS ( ( 4, 4 ),
 ( 2, 2 ),
 ( 0.000000000000000000, 1.000000000000000000 ),
 ( 0.000000000000000000, 1.000000000000000000 ),
 .UNSPECIFIED. ) 
 GEOMETRIC_REPRESENTATION_ITEM ( )  RATIONAL_B_SPLINE_SURFACE ( (
 ( 1.000000000000000000, 1.000000000000000000),
 ( 0.9593108457356467333, 0.9995965569486454649),
 ( 0.9593108457356467333, 0.9995965569486454649),
 ( 1.000000000000000000, 1.000000000000000000) ) ) 
 REPRESENTATION_ITEM ( '' )  SURFACE ( )  );
#8565 = LINE ( 'NONE', #1399, #4414 ) ;
#8566 = ADVANCED_FACE ( 'NONE', ( #1589 ), #7243, .T. ) ;
#8567 = CARTESIAN_POINT ( 'NONE',  ( 1.861706995891673433, -0.5394761475744983548, -12.44571539481144562 ) ) ;
#8568 = CARTESIAN_POINT ( 'NONE',  ( 0.3137051932979757485, 7.698472063774634222, -11.37800749014122736 ) ) ;
#8569 = ORIENTED_EDGE ( 'NONE', *, *, #7259, .F. ) ;
#8570 = CARTESIAN_POINT ( 'NONE',  ( 0.4862570985993252548, 5.003653737315486794, 12.97920246947881395 ) ) ;
#8571 = LINE ( 'NONE', #12961, #18134 ) ;
#8572 = CIRCLE ( 'NONE', #6038, 14.54644660717763927 ) ;
#8573 = CARTESIAN_POINT ( 'NONE',  ( 2.037104019874286465, 6.699095661347369557, -11.99999999578282406 ) ) ;
#8574 = CARTESIAN_POINT ( 'NONE',  ( 0.000000000000000000, 0.000000000000000000, -3.000000000000000000 ) ) ;
#8575 = EDGE_CURVE ( 'NONE', #18014, #14303, #11350, .T. ) ;
#8576 = DIRECTION ( 'NONE',  ( 1.444447458290427415E-30, 5.204170427930420297E-16, 1.000000000000000000 ) ) ;
#8577 = CARTESIAN_POINT ( 'NONE',  ( 16.58200780006414732, 0.002844973367391037070, 0.01080144354108989249 ) ) ;
#8578 = PLANE ( 'NONE',  #8284 ) ;
#8579 = DIRECTION ( 'NONE',  ( 0.000000000000000000, 0.000000000000000000, 1.000000000000000000 ) ) ;
#8580 = ORIENTED_EDGE ( 'NONE', *, *, #1607, .T. ) ;
#8581 = ORIENTED_EDGE ( 'NONE', *, *, #6846, .T. ) ;
#8582 = FACE_OUTER_BOUND ( 'NONE', #14177, .T. ) ;
#8583 = VERTEX_POINT ( 'NONE', #1301 ) ;
#8584 = ORIENTED_EDGE ( 'NONE', *, *, #11096, .T. ) ;
#8585 = EDGE_CURVE ( 'NONE', #11329, #1566, #17167, .T. ) ;
#8586 = CARTESIAN_POINT ( 'NONE',  ( 0.4754618798421162973, -3.583352865732763792, 13.45049478164058776 ) ) ;
#8587 = VERTEX_POINT ( 'NONE', #10289 ) ;
#8588 = CARTESIAN_POINT ( 'NONE',  ( 1.560000000000000053, 0.8660254037844389297, 1.500000000000000000 ) ) ;
#8589 = EDGE_CURVE ( 'NONE', #15501, #1561, #4181, .T. ) ;
#8590 = EDGE_CURVE ( 'NONE', #13735, #12765, #17555, .T. ) ;
#8591 = DIRECTION ( 'NONE',  ( 0.000000000000000000, 0.000000000000000000, 1.000000000000000000 ) ) ;
#8592 = CARTESIAN_POINT ( 'NONE',  ( 16.56822296793089322, -0.009847136207495329335, 0.002414375228568802195 ) ) ;
#8593 = FACE_OUTER_BOUND ( 'NONE', #13210, .T. ) ;
#8594 = ORIENTED_EDGE ( 'NONE', *, *, #13444, .T. ) ;
#8595 = CARTESIAN_POINT ( 'NONE',  ( 2.002547531651519996, 6.845637710436190737, 10.57595306287294612 ) ) ;
#8596 = LINE ( 'NONE', #9929, #1022 ) ;
#8597 = CARTESIAN_POINT ( 'NONE',  ( 1.847380140988738262, 12.44273713935591097, -0.1101766933249076624 ) ) ;
#8598 = FACE_OUTER_BOUND ( 'NONE', #105, .T. ) ;
#8599 = EDGE_CURVE ( 'NONE', #14131, #14913, #2964, .T. ) ;
#8600 = CARTESIAN_POINT ( 'NONE',  ( 0.3939875929385667219, -3.598491969338320384, 13.34133634968953785 ) ) ;
#8601 = PLANE ( 'NONE',  #5006 ) ;
#8602 = EDGE_CURVE ( 'NONE', #9114, #3538, #16187, .T. ) ;
#8603 = CARTESIAN_POINT ( 'NONE',  ( 0.000000000000000000, -35.00000000000000000, -3.000000000000000000 ) ) ;
#8604 = CYLINDRICAL_SURFACE ( 'NONE', #16898, 5.000000000000000000 ) ;
#8605 = VERTEX_POINT ( 'NONE', #10189 ) ;
#8606 = VECTOR ( 'NONE', #12033, 1000.000000000000000 ) ;
#8607 = CARTESIAN_POINT ( 'NONE',  ( 3.074695600507274307, 11.23985886659449029, -10.75417554975685341 ) ) ;
#8609 = ORIENTED_EDGE ( 'NONE', *, *, #14362, .T. ) ;
#8608 = CARTESIAN_POINT ( 'NONE',  ( 1.959212340397939123, 6.829000156128186561, 10.53510106265284563 ) ) ;
#8610 = DIRECTION ( 'NONE',  ( -0.7635533937278214944, 0.5347026451755939602, 0.3620487483322503142 ) ) ;
#8611 = CARTESIAN_POINT ( 'NONE',  ( 0.3148208552358935930, -13.13564827777586785, -4.026279359288564841 ) ) ;
#8612 = VERTEX_POINT ( 'NONE', #18687 ) ;
#8613 = CARTESIAN_POINT ( 'NONE',  ( 14.99999999999999289, 15.00000000000000000, 3.000000000000000000 ) ) ;
#8614 = DIRECTION ( 'NONE',  ( -0.000000000000000000, -0.5000000000000003331, -0.8660254037844384856 ) ) ;
#8615 = ORIENTED_EDGE ( 'NONE', *, *, #2528, .F. ) ;
#8616 = CARTESIAN_POINT ( 'NONE',  ( 0.3095370825347234511, 7.700448427571873644, 11.38092634279631277 ) ) ;
#8617 = CARTESIAN_POINT ( 'NONE',  ( 18.75000000000000000, 0.000000000000000000, 0.000000000000000000 ) ) ;
#8618 = CARTESIAN_POINT ( 'NONE',  ( 0.3151926232592506816, -4.172630140040890723, 13.09050869763091107 ) ) ;
#8619 = CARTESIAN_POINT ( 'NONE',  ( 0.4862570985993235340, 11.67702470553376060, -7.559321496869298329 ) ) ;
#8620 = DIRECTION ( 'NONE',  ( -1.000000000000000000, -0.000000000000000000, -0.000000000000000000 ) ) ;
#8621 = ADVANCED_FACE ( 'NONE', ( #1207 ), #17583, .T. ) ;
#8622 =( GEOMETRIC_REPRESENTATION_CONTEXT ( 3 ) GLOBAL_UNCERTAINTY_ASSIGNED_CONTEXT ( ( #15689 ) ) GLOBAL_UNIT_ASSIGNED_CONTEXT ( ( #6212, #3034, #7465 ) ) REPRESENTATION_CONTEXT ( 'NONE', 'WORKASPACE' ) );
#8623 = CARTESIAN_POINT ( 'NONE',  ( -194.9999999999999716, 9.999999999999973355, 6.000000000000000000 ) ) ;
#8624 = EDGE_CURVE ( 'NONE', #12529, #5127, #8765, .T. ) ;
#8625 = CARTESIAN_POINT ( 'NONE',  ( 2.353870697619111940, -12.53036919722786813, 3.268530966681581607 ) ) ;
#8626 = FACE_OUTER_BOUND ( 'NONE', #16779, .T. ) ;
#8627 = CARTESIAN_POINT ( 'NONE',  ( 3.074695600507223681, -13.70113613813211195, -7.366518011946086908 ) ) ;
#8628 = CARTESIAN_POINT ( 'NONE',  ( 0.4385251269669942498, 7.540955776459739468, 11.63205320541525900 ) ) ;
#8629 = APPLICATION_CONTEXT ( 'automotive_design' ) ;
#8630 = ORIENTED_EDGE ( 'NONE', *, *, #5052, .F. ) ;
#8631 = DIRECTION ( 'NONE',  ( 0.000000000000000000, 0.000000000000000000, 1.000000000000000000 ) ) ;
#8632 = CARTESIAN_POINT ( 'NONE',  ( 2.002547531651519996, 6.845637710436341727, -10.57595306287284842 ) ) ;
#8633 = ORIENTED_EDGE ( 'NONE', *, *, #13219, .F. ) ;
#8634 = ORIENTED_EDGE ( 'NONE', *, *, #5662, .T. ) ;
#8635 = CARTESIAN_POINT ( 'NONE',  ( 16.58200780006414732, -0.006043560077721639792, -0.009393638146079824613 ) ) ;
#8636 = EDGE_LOOP ( 'NONE', ( #278, #2824, #15357, #10482 ) ) ;
#8637 = ORIENTED_EDGE ( 'NONE', *, *, #17611, .T. ) ;
#8638 = VECTOR ( 'NONE', #14170, 1000.000000000000114 ) ;
#8639 = CARTESIAN_POINT ( 'NONE',  ( 2.002547531651521773, 9.778737580845699995, 7.942910686618207983 ) ) ;
#8640 = DIRECTION ( 'NONE',  ( 1.000000000000000000, 0.000000000000000000, 0.000000000000000000 ) ) ;
#8641 = CARTESIAN_POINT ( 'NONE',  ( 0.3142011359265323156, -7.762194356530850214, 11.33549115679420538 ) ) ;
#8642 = CARTESIAN_POINT ( 'NONE',  ( 0.8740779401512712710, 11.05257166392075341, -9.070947476926923159 ) ) ;
#8643 = EDGE_CURVE ( 'NONE', #348, #8116, #12994, .T. ) ;
#8644 = ADVANCED_FACE ( 'NONE', ( #7140 ), #10530, .F. ) ;
#8645 = CARTESIAN_POINT ( 'NONE',  ( 0.3137051932979809665, -3.805684345189881856, 13.20008686438104739 ) ) ;
#8646 = EDGE_CURVE ( 'NONE', #13406, #12130, #18036, .T. ) ;
#8647 = CARTESIAN_POINT ( 'NONE',  ( 1.845756295923359769, 10.33914852636104875, 6.920504327368230513 ) ) ;
#8648 = CARTESIAN_POINT ( 'NONE',  ( 0.3150686449036028680, -13.01866258978840030, 4.391272911157273029 ) ) ;
#8649 = CARTESIAN_POINT ( 'NONE',  ( 2.123976203522053741, 6.261444813538558307, 14.31368049382972529 ) ) ;
#8650 = CIRCLE ( 'NONE', #3142, 12.15840553252917289 ) ;
#8651 = VERTEX_POINT ( 'NONE', #16514 ) ;
#8652 = ORIENTED_EDGE ( 'NONE', *, *, #17188, .T. ) ;
#8653 = EDGE_LOOP ( 'NONE', ( #12836, #11603, #10603, #13741 ) ) ;
#8654 = ORIENTED_EDGE ( 'NONE', *, *, #11834, .T. ) ;
#8655 = ORIENTED_EDGE ( 'NONE', *, *, #14180, .T. ) ;
#8656 = CARTESIAN_POINT ( 'NONE',  ( 1.847168016377985333, 3.666915430942765397, -11.89018175117590559 ) ) ;
#8657 = CARTESIAN_POINT ( 'NONE',  ( -2.500000000000000000, 3.061616997868383141E-16, -13.00000000000000533 ) ) ;
#8658 = DIRECTION ( 'NONE',  ( -1.000000000000000000, -0.000000000000000000, -0.000000000000000000 ) ) ;
#8659 = ORIENTED_EDGE ( 'NONE', *, *, #7966, .F. ) ;
#8660 = FACE_OUTER_BOUND ( 'NONE', #13052, .T. ) ;
#8661 = DIRECTION ( 'NONE',  ( 0.000000000000000000, 0.000000000000000000, 1.000000000000000000 ) ) ;
#8662 = CARTESIAN_POINT ( 'NONE',  ( 6.340401435272480235, 2.969608215370613813, -11.99999999980921572 ) ) ;
#8663 = CARTESIAN_POINT ( 'NONE',  ( 5.000000000000000000, 0.000000000000000000, -6.000000000000000000 ) ) ;
#8664 = DIRECTION ( 'NONE',  ( 1.000000000000000000, 0.000000000000000000, 0.000000000000000000 ) ) ;
#8665 = EDGE_CURVE ( 'NONE', #8138, #12327, #2900, .T. ) ;
#8666 = CARTESIAN_POINT ( 'NONE',  ( 1.918921323896323194, 12.08297777410669482, -3.258415356426395793 ) ) ;
#8667 = CARTESIAN_POINT ( 'NONE',  ( 1.846955891736119293, 4.094751675596701723, 11.74973605926565767 ) ) ;
#8668 = EDGE_CURVE ( 'NONE', #5097, #18549, #12762, .T. ) ;
#8669 = LINE ( 'NONE', #13065, #14368 ) ;
#8670 = B_SPLINE_CURVE_WITH_KNOTS ( 'NONE', 3,
 ( #14664, #7323, #1577, #9035, #14472, #4640 ),
 .UNSPECIFIED., .F., .F.,
 ( 4, 2, 4 ),
 ( 0.000000000000000000, 0.001656992708822505175, 0.003313985417645010350 ),
 .UNSPECIFIED. ) ;
#8671 = EDGE_CURVE ( 'NONE', #13313, #5127, #14587, .T. ) ;
#8672 = CARTESIAN_POINT ( 'NONE',  ( 1.847461586945727374, -3.813310247068524284, 11.84459954310609753 ) ) ;
#8673 = ORIENTED_EDGE ( 'NONE', *, *, #2623, .T. ) ;
#8674 =( BOUNDED_SURFACE ( )  B_SPLINE_SURFACE ( 3, 1, ( 
 ( #787, #9295 ),
 ( #878, #6625 ),
 ( #697, #18275 ),
 ( #15400, #15129 ) ),
 .UNSPECIFIED., .F., .F., .T. ) 
 B_SPLINE_SURFACE_WITH_KNOTS ( ( 4, 4 ),
 ( 2, 2 ),
 ( 0.000000000000000000, 1.000000000000000000 ),
 ( 0.000000000000000000, 1.000000000000000000 ),
 .UNSPECIFIED. ) 
 GEOMETRIC_REPRESENTATION_ITEM ( )  RATIONAL_B_SPLINE_SURFACE ( (
 ( 1.000000000000000000, 1.000000000000000000),
 ( 0.9933953342250438912, 0.8357391271907739227),
 ( 0.9933953342250438912, 0.8357391271907739227),
 ( 1.000000000000000000, 1.000000000000000000) ) ) 
 REPRESENTATION_ITEM ( '' )  SURFACE ( )  );
#8675 = ORIENTED_EDGE ( 'NONE', *, *, #18654, .T. ) ;
#8676 = ORIENTED_EDGE ( 'NONE', *, *, #17028, .F. ) ;
#8677 = ORIENTED_EDGE ( 'NONE', *, *, #12308, .F. ) ;
#8678 = CARTESIAN_POINT ( 'NONE',  ( 0.3720661004400037664, 13.79610186261029625, 0.7231997263365286255 ) ) ;
#8679 = CIRCLE ( 'NONE', #2902, 5.000000000000000888 ) ;
#8680 = CIRCLE ( 'NONE', #18166, 5.000000000000000000 ) ;
#8681 = ORIENTED_EDGE ( 'NONE', *, *, #648, .F. ) ;
#8682 = PLANE ( 'NONE',  #14026 ) ;
#8683 = AXIS2_PLACEMENT_3D ( 'NONE', #8119, #13928, #4959 ) ;
#8684 = CARTESIAN_POINT ( 'NONE',  ( 0.000000000000000000, 0.000000000000000000, 0.000000000000000000 ) ) ;
#8685 = DIRECTION ( 'NONE',  ( 0.000000000000000000, 0.000000000000000000, 1.000000000000000000 ) ) ;
#8686 = DIRECTION ( 'NONE',  ( -1.000000000000000000, 0.000000000000000000, 0.000000000000000000 ) ) ;
#8687 = VERTEX_POINT ( 'NONE', #15065 ) ;
#8688 = CARTESIAN_POINT ( 'NONE',  ( 16.56679352167444819, -0.008252760440870528930, -0.004277682826582232013 ) ) ;
#8689 = LINE ( 'NONE', #2663, #15851 ) ;
#8690 = CARTESIAN_POINT ( 'NONE',  ( 0.3142011359265340920, -13.73310835363014348, 0.3830873813805846240 ) ) ;
#8691 = CARTESIAN_POINT ( 'NONE',  ( 0.000000000000000000, 0.000000000000000000, 0.000000000000000000 ) ) ;
#8692 = CARTESIAN_POINT ( 'NONE',  ( 0.3308579732647007887, -8.558831104906994725, 10.76782854710824111 ) ) ;
#8693 = CARTESIAN_POINT ( 'NONE',  ( 1.847034903785822690, 7.126331315909270714, 10.19974412751566994 ) ) ;
#8694 = AXIS2_PLACEMENT_3D ( 'NONE', #18627, #10127, #2665 ) ;
#8695 = AXIS2_PLACEMENT_3D ( 'NONE', #874, #8330, #2391 ) ;
#8696 = DIRECTION ( 'NONE',  ( 0.000000000000000000, 0.000000000000000000, 1.000000000000000000 ) ) ;
#8697 = LINE ( 'NONE', #18827, #15973 ) ;
#8698 = ORIENTED_EDGE ( 'NONE', *, *, #9133, .T. ) ;
#8699 = EDGE_CURVE ( 'NONE', #18618, #6956, #497, .T. ) ;
#8700 = LINE ( 'NONE', #4505, #964 ) ;
#8702 = EDGE_LOOP ( 'NONE', ( #2768, #11372, #17647, #18808 ) ) ;
#8701 = LINE ( 'NONE', #10422, #11203 ) ;
#8703 = CARTESIAN_POINT ( 'NONE',  ( 0.3151926232592472954, 8.013596737356548871, -11.16039997398644879 ) ) ;
#8704 = CARTESIAN_POINT ( 'NONE',  ( 0.4862570985993235340, -0.7479633556563419772, 13.89016912371017121 ) ) ;
#8705 = B_SPLINE_CURVE_WITH_KNOTS ( 'NONE', 3,
 ( #4993, #11212, #2670, #12812, #15402, #14343 ),
 .UNSPECIFIED., .F., .F.,
 ( 4, 2, 4 ),
 ( 0.000000000000000000, 0.001656992708822831520, 0.003313985417645663040 ),
 .UNSPECIFIED. ) ;
#8706 = ORIENTED_EDGE ( 'NONE', *, *, #12548, .F. ) ;
#8707 = FACE_OUTER_BOUND ( 'NONE', #10265, .T. ) ;
#8708 = CONICAL_SURFACE ( 'NONE', #2889, 14.54644660717763927, 0.8559913436420816257 ) ;
#8709 = CARTESIAN_POINT ( 'NONE',  ( 5.783659440659287831, -3.949482697158031463, -11.99999999872349576 ) ) ;
#8710 = AXIS2_PLACEMENT_3D ( 'NONE', #13565, #486, #13277 ) ;
#8711 = B_SPLINE_CURVE_WITH_KNOTS ( 'NONE', 3,
 ( #11274, #18698, #17090, #11450, #6782, #14400 ),
 .UNSPECIFIED., .F., .F.,
 ( 4, 2, 4 ),
 ( 0.000000000000000000, 0.0001828790815886944003, 0.0003657581631773888006 ),
 .UNSPECIFIED. ) ;
#8712 = ORIENTED_EDGE ( 'NONE', *, *, #9889, .T. ) ;
#8713 = CARTESIAN_POINT ( 'NONE',  ( -194.9999999999999716, -45.00000000000003553, 3.000000000000000000 ) ) ;
#8714 = FACE_OUTER_BOUND ( 'NONE', #8336, .T. ) ;
#8715 = EDGE_CURVE ( 'NONE', #16337, #4624, #5, .T. ) ;
#8716 = CARTESIAN_POINT ( 'NONE',  ( 0.3137051932979809665, -4.679953077377580151, 12.91601973349268917 ) ) ;
#8717 = CARTESIAN_POINT ( 'NONE',  ( 0.3150692679895978898, -11.20465057551030874, 7.951395415075045214 ) ) ;
#8718 = ORIENTED_EDGE ( 'NONE', *, *, #8435, .T. ) ;
#8719 = CARTESIAN_POINT ( 'NONE',  ( 16.56679352167444819, 0.004162264567719650525, 0.008311568981097349276 ) ) ;
#8720 = DIRECTION ( 'NONE',  ( -1.000000000000000000, -0.000000000000000000, -0.000000000000000000 ) ) ;
#8721 = VECTOR ( 'NONE', #822, 1000.000000000000114 ) ;
#8722 =( GEOMETRIC_REPRESENTATION_CONTEXT ( 3 ) GLOBAL_UNCERTAINTY_ASSIGNED_CONTEXT ( ( #17601 ) ) GLOBAL_UNIT_ASSIGNED_CONTEXT ( ( #13891, #16682, #6649 ) ) REPRESENTATION_CONTEXT ( 'NONE', 'WORKASPACE' ) );
#8723 = LINE ( 'NONE', #8817, #4381 ) ;
#8724 = CARTESIAN_POINT ( 'NONE',  ( 1.846138399168762989, 4.238866729160403857, 11.69739621335923729 ) ) ;
#8725 = CARTESIAN_POINT ( 'NONE',  ( -30.00000000000000355, -12.50000000000000178, 7.000000000000000000 ) ) ;
#8726 = ORIENTED_EDGE ( 'NONE', *, *, #4981, .T. ) ;
#8727 = CARTESIAN_POINT ( 'NONE',  ( 3.950837973638675393, -10.51028938476210328, -10.05648675950137871 ) ) ;
#8728 = CARTESIAN_POINT ( 'NONE',  ( 3.377929128793385249, 13.64476897106782971, 3.070552481924919253 ) ) ;
#8729 = ORIENTED_EDGE ( 'NONE', *, *, #16515, .T. ) ;
#8730 = ORIENTED_EDGE ( 'NONE', *, *, #18589, .T. ) ;
#8731 = CARTESIAN_POINT ( 'NONE',  ( 16.57210152137263393, 0.003862718596009469003, -0.01402404281923040792 ) ) ;
#8732 = ORIENTED_EDGE ( 'NONE', *, *, #2351, .F. ) ;
#8733 = CARTESIAN_POINT ( 'NONE',  ( 1.959283090834842200, -3.239245055717051791, 12.12982544407804220 ) ) ;
#8734 = ORIENTED_EDGE ( 'NONE', *, *, #428, .F. ) ;
#8735 = EDGE_CURVE ( 'NONE', #10624, #14167, #7330, .T. ) ;
#8736 = CARTESIAN_POINT ( 'NONE',  ( 16.56782317627811096, -0.008141063682853446129, 0.005492611183758502880 ) ) ;
#8737 = AXIS2_PLACEMENT_3D ( 'NONE', #6068, #11897, #17733 ) ;
#8738 = CARTESIAN_POINT ( 'NONE',  ( 1.847247051441596621, -7.448813758297236909, 9.967131402978164800 ) ) ;
#8739 =( GEOMETRIC_REPRESENTATION_CONTEXT ( 3 ) GLOBAL_UNCERTAINTY_ASSIGNED_CONTEXT ( ( #7511 ) ) GLOBAL_UNIT_ASSIGNED_CONTEXT ( ( #607, #9105, #6344 ) ) REPRESENTATION_CONTEXT ( 'NONE', 'WORKASPACE' ) );
#8740 = DIRECTION ( 'NONE',  ( 1.000000000000000000, -0.000000000000000000, -0.000000000000000000 ) ) ;
#8741 = CARTESIAN_POINT ( 'NONE',  ( 0.3145734862173267810, 3.953068532979994831, 13.15783074029279831 ) ) ;
#8742 = ADVANCED_FACE ( 'NONE', ( #3102 ), #11261, .F. ) ;
#8743 = B_SPLINE_CURVE_WITH_KNOTS ( 'NONE', 3,
 ( #4404, #13003, #12816, #7382, #13192, #9185 ),
 .UNSPECIFIED., .F., .F.,
 ( 4, 2, 4 ),
 ( 2.185279341460844539E-18, 0.0002017457492448067953, 0.0004034914984896113680 ),
 .UNSPECIFIED. ) ;
#8744 = DIRECTION ( 'NONE',  ( 0.000000000000000000, 1.000000000000000000, 0.000000000000000000 ) ) ;
#8745 = FACE_OUTER_BOUND ( 'NONE', #4454, .T. ) ;
#8746 = CARTESIAN_POINT ( 'NONE',  ( 5.000000000000000000, 0.000000000000000000, 0.000000000000000000 ) ) ;
#8747 = CARTESIAN_POINT ( 'NONE',  ( 0.3132642857406562342, -10.79548167658028213, -8.495623922778184678 ) ) ;
#8748 = B_SPLINE_CURVE_WITH_KNOTS ( 'NONE', 3,
 ( #391, #3236, #9086, #17981, #6218, #4888 ),
 .UNSPECIFIED., .F., .F.,
 ( 4, 2, 4 ),
 ( 0.000000000000000000, 0.001656992708822033113, 0.003313985417644066227 ),
 .UNSPECIFIED. ) ;
#8749 = CARTESIAN_POINT ( 'NONE',  ( -194.9999999999999716, 4.999999999999973355, 6.000000000000005329 ) ) ;
#8750 = AXIS2_PLACEMENT_3D ( 'NONE', #4762, #17861, #14982 ) ;
#8751 = CARTESIAN_POINT ( 'NONE',  ( 3.512766787570810845, 10.40533104696146083, -10.87507422923874856 ) ) ;
#8752 = ORIENTED_EDGE ( 'NONE', *, *, #10473, .F. ) ;
#8753 = COLOUR_RGB ( '', 0.09019608, 0.27058824, 0.51372549) ;
#8754 = ORIENTED_EDGE ( 'NONE', *, *, #3240, .T. ) ;
#8755 = CIRCLE ( 'NONE', #536, 2.499999999999992006 ) ;
#8756 = ORIENTED_EDGE ( 'NONE', *, *, #18267, .T. ) ;
#8757 = ORIENTED_EDGE ( 'NONE', *, *, #13691, .F. ) ;
#8758 = EDGE_LOOP ( 'NONE', ( #9407, #14108, #6423, #13729 ) ) ;
#8759 = ADVANCED_FACE ( 'NONE', ( #14968 ), #10684, .F. ) ;
#8760 = EDGE_CURVE ( 'NONE', #6081, #13735, #12210, .T. ) ;
#8761 = CARTESIAN_POINT ( 'NONE',  ( 1.845755665166725734, -11.97169564665393970, 3.386720041070682363 ) ) ;
#8762 = CIRCLE ( 'NONE', #7875, 16.06066017081991149 ) ;
#8763 = CARTESIAN_POINT ( 'NONE',  ( 0.3095370825347224519, 13.73357284481724783, 0.4597470195090653799 ) ) ;
#8764 = B_SPLINE_CURVE_WITH_KNOTS ( 'NONE', 3,
 ( #13356, #6100, #16130, #3012 ),
 .UNSPECIFIED., .F., .F.,
 ( 4, 4 ),
 ( 0.000000000000000000, 0.002004993803842603211 ),
 .UNSPECIFIED. ) ;
#8765 = LINE ( 'NONE', #7051, #10579 ) ;
#8766 = ORIENTED_EDGE ( 'NONE', *, *, #2727, .F. ) ;
#8767 = CARTESIAN_POINT ( 'NONE',  ( 1.254009781011409919, 5.487405433548389055, 13.61532727684416955 ) ) ;
#8768 = CIRCLE ( 'NONE', #10929, 5.315148208181397216 ) ;
#8769 = VECTOR ( 'NONE', #16485, 1000.000000000000114 ) ;
#8770 = CARTESIAN_POINT ( 'NONE',  ( 2.636624412714237309, 11.10302021257826866, 11.60464335004050973 ) ) ;
#8771 = DIRECTION ( 'NONE',  ( -0.7635533937278216055, -0.6204116510013465424, -0.1790966170213987851 ) ) ;
#8772 = DIRECTION ( 'NONE',  ( -1.000000000000000000, 0.000000000000000000, 0.000000000000000000 ) ) ;
#8773 = DIRECTION ( 'NONE',  ( 0.7071067818211358436, 8.659560554583467185E-17, 0.7071067805519591909 ) ) ;
#8774 = CARTESIAN_POINT ( 'NONE',  ( 0.000000000000000000, 0.000000000000000000, 0.000000000000000000 ) ) ;
#8775 = CARTESIAN_POINT ( 'NONE',  ( 2.320521194582657376, -3.126729093671833937, 15.43440938317077915 ) ) ;
#8776 = DIRECTION ( 'NONE',  ( 1.000000000000000000, 1.577021341797097560E-16, -0.000000000000000000 ) ) ;
#8777 = ORIENTED_EDGE ( 'NONE', *, *, #1372, .T. ) ;
#8778 = ORIENTED_EDGE ( 'NONE', *, *, #10675, .T. ) ;
#8779 = ORIENTED_EDGE ( 'NONE', *, *, #1423, .T. ) ;
#8780 = ORIENTED_EDGE ( 'NONE', *, *, #8017, .F. ) ;
#8781 = CARTESIAN_POINT ( 'NONE',  ( 16.56872352241294521, 0.009382111268606257298, -0.004564908236400254740 ) ) ;
#8782 = EDGE_CURVE ( 'NONE', #12877, #1860, #5018, .T. ) ;
#8783 = ORIENTED_EDGE ( 'NONE', *, *, #2654, .F. ) ;
#8784 = ADVANCED_FACE ( 'NONE', ( #12658 ), #15341, .T. ) ;
#8785 = CARTESIAN_POINT ( 'NONE',  ( 8.522092701127531811, -5.841710761610158009, 3.777034505568503064 ) ) ;
#8786 = DIRECTION ( 'NONE',  ( 0.000000000000000000, 0.000000000000000000, 1.000000000000000000 ) ) ;
#8787 = CARTESIAN_POINT ( 'NONE',  ( 3.950837973638668288, 0.000000000000000000, 0.000000000000000000 ) ) ;
#8788 = CARTESIAN_POINT ( 'NONE',  ( 1.959283090834841090, -12.12982544407802799, -3.239245055717093091 ) ) ;
#8789 = EDGE_LOOP ( 'NONE', ( #3369, #232, #8200, #13923, #11668, #2123 ) ) ;
#8790 = CARTESIAN_POINT ( 'NONE',  ( 3.664313757352971823, 7.012524439851495650, 12.42002390572628201 ) ) ;
#8791 = AXIS2_PLACEMENT_3D ( 'NONE', #12465, #6919, #16861 ) ;
#8792 = CARTESIAN_POINT ( 'NONE',  ( 3.950837973638675393, 10.51028938476217967, 10.05648675950130233 ) ) ;
#8793 = DIRECTION ( 'NONE',  ( 0.000000000000000000, 0.000000000000000000, -1.000000000000000000 ) ) ;
#8794 = CARTESIAN_POINT ( 'NONE',  ( 0.3137051932979792457, 4.679953077377670745, -12.91601973349265720 ) ) ;
#8795 = CARTESIAN_POINT ( 'NONE',  ( 2.002547531651519996, 11.75462648437108015, -4.532360870844206246 ) ) ;
#8796 = CARTESIAN_POINT ( 'NONE',  ( 0.000000000000000000, 2.499999999999998668, -16.99999999999999645 ) ) ;
#8797 = ORIENTED_EDGE ( 'NONE', *, *, #2290, .T. ) ;
#8798 = CARTESIAN_POINT ( 'NONE',  ( 0.4862570985993235340, -11.67702470553370553, 7.559321496869385371 ) ) ;
#8800 = ORIENTED_EDGE ( 'NONE', *, *, #18240, .F. ) ;
#8799 = FACE_OUTER_BOUND ( 'NONE', #2438, .T. ) ;
#8801 = CARTESIAN_POINT ( 'NONE',  ( 1.959283090834842644, 12.12982544407805108, 3.239245055717007826 ) ) ;
#8802 = DIRECTION ( 'NONE',  ( 1.000000000000000000, 0.000000000000000000, 0.000000000000000000 ) ) ;
#8803 = ORIENTED_EDGE ( 'NONE', *, *, #18181, .T. ) ;
#8804 = CARTESIAN_POINT ( 'NONE',  ( 0.3150692679895985560, 4.391039771493846722, -13.01874238516605331 ) ) ;
#8805 = CARTESIAN_POINT ( 'NONE',  ( 1.461502493107205369, -7.499999999999999112, -13.09494173305809817 ) ) ;
#8806 = EDGE_LOOP ( 'NONE', ( #15947, #7111, #15982, #8020 ) ) ;
#8807 = CARTESIAN_POINT ( 'NONE',  ( 0.3170788640506441158, 13.11595226728158003, 4.100430649998006771 ) ) ;
#8808 = CARTESIAN_POINT ( 'NONE',  ( 3.950837973638675393, -6.888253895133384930, 12.81214529934972823 ) ) ;
#8809 = EDGE_CURVE ( 'NONE', #5121, #6854, #5663, .T. ) ;
#8810 = CARTESIAN_POINT ( 'NONE',  ( 1.846138399168762101, 4.238866729160568170, -11.69739621335917690 ) ) ;
#8811 = CARTESIAN_POINT ( 'NONE',  ( 0.3132642857406524040, 3.740125687984731773, 13.21852905223340535 ) ) ;
#8812 = ADVANCED_FACE ( 'NONE', ( #732 ), #6564, .T. ) ;
#8813 = CONTEXT_DEPENDENT_SHAPE_REPRESENTATION ( #6943, #16557 ) ;
#8814 = EDGE_CURVE ( 'NONE', #4000, #6301, #2169, .T. ) ;
#8815 = CARTESIAN_POINT ( 'NONE',  ( 0.3058872367615226295, 13.24582953854930345, -3.664492643742625511 ) ) ;
#8816 = CARTESIAN_POINT ( 'NONE',  ( 0.4384471787762801442, 10.76632603192799742, -8.732395932355569101 ) ) ;
#8817 = CARTESIAN_POINT ( 'NONE',  ( -205.0000000000000000, 4.999999999999974243, -153.7432847437423789 ) ) ;
#8818 = CARTESIAN_POINT ( 'NONE',  ( 3.353306896162454809, 12.02594772223106645, -7.069984850384678055 ) ) ;
#8819 = CARTESIAN_POINT ( 'NONE',  ( 22.75000000000000000, 2.516649172247811061E-16, -2.055000000000000160 ) ) ;
#8820 = ORIENTED_EDGE ( 'NONE', *, *, #3651, .T. ) ;
#8821 = FACE_OUTER_BOUND ( 'NONE', #17980, .T. ) ;
#8822 = CARTESIAN_POINT ( 'NONE',  ( 3.950837973638675393, 6.888253895133292559, 12.81214529934977797 ) ) ;
#8823 = EDGE_LOOP ( 'NONE', ( #11004, #12491, #6029, #6953 ) ) ;
#8824 = ORIENTED_EDGE ( 'NONE', *, *, #3042, .F. ) ;
#8825 = CARTESIAN_POINT ( 'NONE',  ( 16.56753206892534891, 0.008490833999798002782, -0.004253784598196794220 ) ) ;
#8826 = ORIENTED_EDGE ( 'NONE', *, *, #6019, .F. ) ;
#8827 = CARTESIAN_POINT ( 'NONE',  ( 16.57210152137263393, -0.01136813053532154116, 0.009075239946109162070 ) ) ;
#8828 = AXIS2_PLACEMENT_3D ( 'NONE', #14997, #1818, #4778 ) ;
#8829 = EDGE_CURVE ( 'NONE', #2882, #6105, #18394, .T. ) ;
#8830 = CIRCLE ( 'NONE', #6405, 1.500000000000000000 ) ;
#8831 = VERTEX_POINT ( 'NONE', #914 ) ;
#8832 = CARTESIAN_POINT ( 'NONE',  ( -194.9999999999999716, 4.999999999999973355, 6.000000000000000000 ) ) ;
#8833 = EDGE_CURVE ( 'NONE', #6154, #9401, #18484, .T. ) ;
#8834 = EDGE_CURVE ( 'NONE', #5568, #17620, #10750, .T. ) ;
#8835 = CARTESIAN_POINT ( 'NONE',  ( 1.846822687350024417, -7.547953575784189795, 9.891732594446548177 ) ) ;
#8836 = FACE_OUTER_BOUND ( 'NONE', #13635, .T. ) ;
#8837 = CARTESIAN_POINT ( 'NONE',  ( 1.136782529653004747, -40.00000000000000000, 6.000000000000000000 ) ) ;
#8838 = UNCERTAINTY_MEASURE_WITH_UNIT (LENGTH_MEASURE( 1.000000000000000082E-05 ), #13694, 'distance_accuracy_value', 'NONE');
#8839 = CARTESIAN_POINT ( 'NONE',  ( 1.918918678667045352, 9.738328798462491775, -7.860057224348732774 ) ) ;
#8840 = CARTESIAN_POINT ( 'NONE',  ( 0.3095370825347224519, -0.4597470195089233824, -13.73357284481725316 ) ) ;
#8841 = CARTESIAN_POINT ( 'NONE',  ( 1.342453679581834924, -14.76648944001040142, 0.9602753779830212055 ) ) ;
#8842 = CARTESIAN_POINT ( 'NONE',  ( 2.369999999999999662, 0.000000000000000000, 4.750000000000000000 ) ) ;
#8843 = ORIENTED_EDGE ( 'NONE', *, *, #2244, .F. ) ;
#8844 = DIRECTION ( 'NONE',  ( -1.000000000000000000, -0.000000000000000000, -0.000000000000000000 ) ) ;
#8845 = CARTESIAN_POINT ( 'NONE',  ( 0.3150692679895987780, 13.73846569174797061, 0.1531143455845020152 ) ) ;
#8846 = EDGE_CURVE ( 'NONE', #8095, #2099, #5918, .T. ) ;
#8847 = CARTESIAN_POINT ( 'NONE',  ( 0.4754618798421162973, 0.7484603771384427118, 13.89949764182683012 ) ) ;
#8848 = EDGE_LOOP ( 'NONE', ( #4914, #10747, #1802, #7893 ) ) ;
#8849 = ORIENTED_EDGE ( 'NONE', *, *, #16965, .F. ) ;
#8850 = ORIENTED_EDGE ( 'NONE', *, *, #10375, .F. ) ;
#8851 = ORIENTED_EDGE ( 'NONE', *, *, #12485, .F. ) ;
#8852 = CYLINDRICAL_SURFACE ( 'NONE', #11405, 2.500000000000000000 ) ;
#8853 = LINE ( 'NONE', #1588, #18462 ) ;
#8854 = CARTESIAN_POINT ( 'NONE',  ( 1.977436885025011470, 11.52792723756289206, 10.21547824869447219 ) ) ;
#8855 = ORIENTED_EDGE ( 'NONE', *, *, #10809, .T. ) ;
#8856 = DIRECTION ( 'NONE',  ( -0.000000000000000000, -0.000000000000000000, 1.000000000000000000 ) ) ;
#8857 = CARTESIAN_POINT ( 'NONE',  ( 0.3132635586635977853, -11.41586812343484070, -7.641727604904016147 ) ) ;
#8858 = CARTESIAN_POINT ( 'NONE',  ( 2.320520222538116961, 10.64885284335071169, -11.60169517779341852 ) ) ;
#8859 = CYLINDRICAL_SURFACE ( 'NONE', #13768, 1.000000000000000000 ) ;
#8860 = CARTESIAN_POINT ( 'NONE',  ( 0.000000000000000000, 0.000000000000000000, 7.000000000000000000 ) ) ;
#8861 = DIRECTION ( 'NONE',  ( -1.000000000000000000, 0.000000000000000000, -0.000000000000000000 ) ) ;
#8862 = CARTESIAN_POINT ( 'NONE',  ( 3.074695600507765025, 15.30693405987741684, -2.772091048738999142 ) ) ;
#8863 = CARTESIAN_POINT ( 'NONE',  ( 0.4862570985993252548, -12.97920246947875889, -5.003653737315625349 ) ) ;
#8864 = B_SPLINE_CURVE_WITH_KNOTS ( 'NONE', 3,
 ( #6347, #15028, #5629, #2480, #8608, #15869 ),
 .UNSPECIFIED., .F., .F.,
 ( 4, 2, 4 ),
 ( 0.000000000000000000, 0.0001828790815886947255, 0.0003657581631773894511 ),
 .UNSPECIFIED. ) ;
#8865 = CARTESIAN_POINT ( 'NONE',  ( 1.846955891736116184, 7.525208385419960067, 9.909315188408065467 ) ) ;
#8866 = EDGE_CURVE ( 'NONE', #8048, #13856, #15257, .T. ) ;
#8867 = ORIENTED_EDGE ( 'NONE', *, *, #16587, .F. ) ;
#8868 = ORIENTED_EDGE ( 'NONE', *, *, #16502, .T. ) ;
#8869 = ORIENTED_EDGE ( 'NONE', *, *, #16854, .T. ) ;
#8870 = ORIENTED_EDGE ( 'NONE', *, *, #8866, .T. ) ;
#8871 = CARTESIAN_POINT ( 'NONE',  ( 2.747332970342022840, 7.289199830147313541, -14.63517873738939379 ) ) ;
#8872 = ORIENTED_EDGE ( 'NONE', *, *, #10675, .F. ) ;
#8873 = CARTESIAN_POINT ( 'NONE',  ( 20.00000000000000711, -45.00000000000000000, 6.000000000000000000 ) ) ;
#8874 = CARTESIAN_POINT ( 'NONE',  ( 16.56679352167444819, 0.009190982326619719436, 0.001390132774594471984 ) ) ;
#8875 = CYLINDRICAL_SURFACE ( 'NONE', #17217, 5.000000000000000000 ) ;
#8876 = CARTESIAN_POINT ( 'NONE',  ( 1.846138399168762101, -11.95493567637848109, -3.446241763653124401 ) ) ;
#8877 = EDGE_LOOP ( 'NONE', ( #12837, #1953, #15406, #1958, #10718 ) ) ;
#8878 = CARTESIAN_POINT ( 'NONE',  ( -2.117556820461446332, 7.500000000000000000, -15.34001259936770545 ) ) ;
#8879 = CARTESIAN_POINT ( 'NONE',  ( 0.3142011359265305392, -4.608101617236689762, -12.94258167753017297 ) ) ;
#8880 = CARTESIAN_POINT ( 'NONE',  ( 16.57210152137263393, 0.01361613799508855013, 0.005118120558001428358 ) ) ;
#8881 = CARTESIAN_POINT ( 'NONE',  ( 1.977228804423517117, 14.12033626431153444, -6.152949558602713864 ) ) ;
#8882 = EDGE_CURVE ( 'NONE', #17181, #15162, #9702, .T. ) ;
#8883 = DIRECTION ( 'NONE',  ( -1.000000000000000000, 0.000000000000000000, -1.335737076501871514E-14 ) ) ;
#8884 = EDGE_CURVE ( 'NONE', #15501, #10168, #6173, .T. ) ;
#8885 = EDGE_CURVE ( 'NONE', #4825, #5275, #12692, .T. ) ;
#8886 = VERTEX_POINT ( 'NONE', #18669 ) ;
#8887 = CARTESIAN_POINT ( 'NONE',  ( 3.074695600507311610, 2.772091048739249164, 15.30693405987785916 ) ) ;
#8889 = ORIENTED_EDGE ( 'NONE', *, *, #10739, .T. ) ;
#8888 = CARTESIAN_POINT ( 'NONE',  ( 1.560000000000000053, 0.8660254037844389297, 1.500000000000000000 ) ) ;
#8890 = CARTESIAN_POINT ( 'NONE',  ( 16.56753206892534891, 0.004368917149005333185, 0.008432171035096464387 ) ) ;
#8891 = DIRECTION ( 'NONE',  ( -1.000000000000000000, -0.000000000000000000, -0.000000000000000000 ) ) ;
#8892 = VERTEX_POINT ( 'NONE', #2703 ) ;
#8893 = DIRECTION ( 'NONE',  ( -1.000000000000000000, 0.000000000000000000, 0.000000000000000000 ) ) ;
#8894 = CARTESIAN_POINT ( 'NONE',  ( -33.49999999999999289, -12.50000000000000178, 6.500000000000000888 ) ) ;
#8895 = EDGE_CURVE ( 'NONE', #12474, #11305, #13236, .T. ) ;
#8896 = ORIENTED_EDGE ( 'NONE', *, *, #16392, .T. ) ;
#8897 = CARTESIAN_POINT ( 'NONE',  ( 16.56753206892534891, -0.006669401563385243120, -0.006760771273035091553 ) ) ;
#8898 = DIRECTION ( 'NONE',  ( 0.000000000000000000, 0.000000000000000000, -1.000000000000000000 ) ) ;
#8899 = DIRECTION ( 'NONE',  ( 0.7561779333270775005, 0.1688126975276512953, 0.6322161072786960379 ) ) ;
#8900 = LINE ( 'NONE', #16172, #7808 ) ;
#8901 = ORIENTED_EDGE ( 'NONE', *, *, #546, .T. ) ;
#8902 = AXIS2_PLACEMENT_3D ( 'NONE', #11649, #3121, #5608 ) ;
#8903 =( NAMED_UNIT ( * ) SI_UNIT ( $, .STERADIAN. ) SOLID_ANGLE_UNIT ( ) );
#8904 = CARTESIAN_POINT ( 'NONE',  ( 3.950837973638675393, -14.31366178983251380, -2.591948120961955926 ) ) ;
#8905 = CARTESIAN_POINT ( 'NONE',  ( 3.950837973638677170, -14.31366178983255466, 2.591948120961746760 ) ) ;
#8906 = EDGE_CURVE ( 'NONE', #2339, #16009, #7029, .T. ) ;
#8907 = CARTESIAN_POINT ( 'NONE',  ( 0.4754618798421162973, -13.45049478164057177, -3.583352865732810866 ) ) ;
#8908 = CARTESIAN_POINT ( 'NONE',  ( 2.123976203522053741, 1.531817366691752502, 15.54801196254787676 ) ) ;
#8909 = DIRECTION ( 'NONE',  ( 2.891205793294679312E-16, 1.000000000000000000, 0.000000000000000000 ) ) ;
#8910 = EDGE_CURVE ( 'NONE', #13343, #137, #5981, .T. ) ;
#8911 = ORIENTED_EDGE ( 'NONE', *, *, #2465, .F. ) ;
#8912 = CARTESIAN_POINT ( 'NONE',  ( 0.3150686449036039227, -7.951193823202478583, 11.20479228691394979 ) ) ;
#8913 = FACE_OUTER_BOUND ( 'NONE', #16164, .T. ) ;
#8914 = ORIENTED_EDGE ( 'NONE', *, *, #12222, .T. ) ;
#8915 = ORIENTED_EDGE ( 'NONE', *, *, #1710, .F. ) ;
#8916 = LINE ( 'NONE', #2698, #17184 ) ;
#8917 = EDGE_LOOP ( 'NONE', ( #128, #9718, #11986 ) ) ;
#8918 = DIRECTION ( 'NONE',  ( -1.000000000000000000, 0.000000000000000000, 0.000000000000000000 ) ) ;
#8919 = CIRCLE ( 'NONE', #5853, 1.000000000000000000 ) ;
#8920 = ORIENTED_EDGE ( 'NONE', *, *, #6572, .T. ) ;
#8921 = EDGE_CURVE ( 'NONE', #11883, #14584, #9651, .T. ) ;
#8922 = CARTESIAN_POINT ( 'NONE',  ( 1.847247051441589960, 10.16425585218611083, -7.177495230324590025 ) ) ;
#8923 = CARTESIAN_POINT ( 'NONE',  ( 3.686287386450715076E-15, -16.60000000000000142, 25.01316734529526187 ) ) ;
#8924 = B_SPLINE_CURVE_WITH_KNOTS ( 'NONE', 3,
 ( #2885, #38, #7412, #15548, #8298, #11266 ),
 .UNSPECIFIED., .F., .F.,
 ( 4, 2, 4 ),
 ( 1.084202172485504434E-19, 0.001657017934709843158, 0.003314035869419686316 ),
 .UNSPECIFIED. ) ;
#8925 = LINE ( 'NONE', #14853, #2918 ) ;
#8926 = CARTESIAN_POINT ( 'NONE',  ( -55.93192566395838128, 4.999999999999974243, 3.000000000000000000 ) ) ;
#8927 = CARTESIAN_POINT ( 'NONE',  ( 0.3151928479966097374, 0.000000000000000000, -13.73922861026898623 ) ) ;
#8928 = DIRECTION ( 'NONE',  ( 0.000000000000000000, 0.000000000000000000, -1.000000000000000000 ) ) ;
#8929 = FACE_OUTER_BOUND ( 'NONE', #17525, .T. ) ;
#8930 = CARTESIAN_POINT ( 'NONE',  ( 3.950837973638675393, -10.05648675950118509, -10.51028938476228980 ) ) ;
#8931 = CARTESIAN_POINT ( 'NONE',  ( 0.3095370825347224519, -10.84046130709064570, 8.444334731363969837 ) ) ;
#8932 = DIRECTION ( 'NONE',  ( -0.000000000000000000, -0.000000000000000000, -1.000000000000000000 ) ) ;
#8933 = CARTESIAN_POINT ( 'NONE',  ( 1.847380140988740260, -11.79969976631074680, 3.949801494731721263 ) ) ;
#8934 = CARTESIAN_POINT ( 'NONE',  ( 0.3095370825347234511, -0.4597470195091165057, 13.73357284481724605 ) ) ;
#8935 = VERTEX_POINT ( 'NONE', #1191 ) ;
#8936 = VECTOR ( 'NONE', #717, 1000.000000000000000 ) ;
#8937 = VERTEX_POINT ( 'NONE', #8639 ) ;
#8938 = B_SPLINE_CURVE_WITH_KNOTS ( 'NONE', 3,
 ( #13055, #259, #17553, #7340 ),
 .UNSPECIFIED., .F., .F.,
 ( 4, 4 ),
 ( 1.524041208624749586E-16, 0.002004993803842462265 ),
 .UNSPECIFIED. ) ;
#8939 = ORIENTED_EDGE ( 'NONE', *, *, #15150, .F. ) ;
#8940 = ORIENTED_EDGE ( 'NONE', *, *, #12536, .F. ) ;
#8941 = B_SPLINE_CURVE_WITH_KNOTS ( 'NONE', 3,
 ( #7379, #13189, #201, #7087, #6034, #4600, #17397, #8703, #7473, #11767, #12998, #18833, #10425 ),
 .UNSPECIFIED., .F., .F.,
 ( 4, 3, 3, 3, 4 ),
 ( 2.453269466693398698E-18, 0.0002299780670421020532, 0.0004599561239687888735, 0.0006896788984287890393, 0.0009194956271626411473 ),
 .UNSPECIFIED. ) ;
#8942 = EDGE_CURVE ( 'NONE', #6378, #17649, #3854, .T. ) ;
#8943 = FACE_OUTER_BOUND ( 'NONE', #8806, .T. ) ;
#8944 = DIRECTION ( 'NONE',  ( 0.000000000000000000, 0.000000000000000000, -1.000000000000000000 ) ) ;
#8945 = CARTESIAN_POINT ( 'NONE',  ( 0.3137051932979775248, 0.4596302728639756197, 13.73004976592202198 ) ) ;
#8946 = ORIENTED_EDGE ( 'NONE', *, *, #1979, .F. ) ;
#8947 = CARTESIAN_POINT ( 'NONE',  ( 1.560000000000000053, -0.8660254037844384856, 1.500000000000000000 ) ) ;
#8948 = EDGE_CURVE ( 'NONE', #11387, #846, #4456, .T. ) ;
#8949 = CARTESIAN_POINT ( 'NONE',  ( 0.000000000000000000, 0.000000000000000000, 0.000000000000000000 ) ) ;
#8950 = CIRCLE ( 'NONE', #13835, 2.700000000000000178 ) ;
#8951 = CARTESIAN_POINT ( 'NONE',  ( 2.636624412714237309, 15.91454522070173638, -2.161493821596664144 ) ) ;
#8952 = CARTESIAN_POINT ( 'NONE',  ( 19.99999999999999645, 15.00000000000000000, 3.000000000000000000 ) ) ;
#8953 = CARTESIAN_POINT ( 'NONE',  ( 0.8740779401510758717, -0.8420120399581221271, -14.27348745891595172 ) ) ;
#8954 = CIRCLE ( 'NONE', #3455, 5.000000000000000888 ) ;
#8955 = CIRCLE ( 'NONE', #4698, 5.000000000000000888 ) ;
#8956 = CARTESIAN_POINT ( 'NONE',  ( 1.847034903785823579, 11.90269060117939048, -3.625649561595184700 ) ) ;
#8957 = CARTESIAN_POINT ( 'NONE',  ( 16.56753206892534891, 0.004253784598196760393, 0.008490833999798020129 ) ) ;
#8958 = LINE ( 'NONE', #14689, #5519 ) ;
#8959 =( BOUNDED_SURFACE ( )  B_SPLINE_SURFACE ( 3, 1, ( 
 ( #6624, #16477 ),
 ( #4905, #786 ),
 ( #4813, #12442 ),
 ( #4715, #10545 ) ),
 .UNSPECIFIED., .F., .F., .T. ) 
 B_SPLINE_SURFACE_WITH_KNOTS ( ( 4, 4 ),
 ( 2, 2 ),
 ( 0.000000000000000000, 1.000000000000000000 ),
 ( 0.000000000000000000, 1.000000000000000000 ),
 .UNSPECIFIED. ) 
 GEOMETRIC_REPRESENTATION_ITEM ( )  RATIONAL_B_SPLINE_SURFACE ( (
 ( 1.000000000000000000, 1.000000000000000000),
 ( 0.9933953342250438912, 0.8357391271907739227),
 ( 0.9933953342250438912, 0.8357391271907739227),
 ( 1.000000000000000000, 1.000000000000000000) ) ) 
 REPRESENTATION_ITEM ( '' )  SURFACE ( )  );
#8960 = VERTEX_POINT ( 'NONE', #1279 ) ;
#8961 = VERTEX_POINT ( 'NONE', #15708 ) ;
#8962 = ORIENTED_EDGE ( 'NONE', *, *, #3412, .F. ) ;
#8963 = EDGE_LOOP ( 'NONE', ( #10870, #6484, #7839, #10014 ) ) ;
#8964 = CARTESIAN_POINT ( 'NONE',  ( 0.4754618798421167414, 5.007009103465430044, -12.98792082933639058 ) ) ;
#8965 = EDGE_CURVE ( 'NONE', #11688, #6836, #10074, .T. ) ;
#8966 = ORIENTED_EDGE ( 'NONE', *, *, #15267, .T. ) ;
#8967 = CARTESIAN_POINT ( 'NONE',  ( 3.664313757352975820, -10.50730552161225972, -9.645155442698879256 ) ) ;
#8968 = AXIS2_PLACEMENT_3D ( 'NONE', #8976, #16348, #7659 ) ;
#8969 = PRESENTATION_LAYER_ASSIGNMENT (  '', '', ( #17798 ) ) ;
#8970 = CARTESIAN_POINT ( 'NONE',  ( -30.00000000000000355, -12.50000000000000178, 0.000000000000000000 ) ) ;
#8971 = CARTESIAN_POINT ( 'NONE',  ( 2.320521194583479829, -10.64885423995220393, -11.60169518685964363 ) ) ;
#8972 = FACE_OUTER_BOUND ( 'NONE', #12206, .T. ) ;
#8973 = ORIENTED_EDGE ( 'NONE', *, *, #1241, .F. ) ;
#8974 = CARTESIAN_POINT ( 'NONE',  ( 0.6933513387705728670, 7.500000000000000888, -14.36029122898768939 ) ) ;
#8975 = ADVANCED_FACE ( 'NONE', ( #15807 ), #2886, .F. ) ;
#8976 = CARTESIAN_POINT ( 'NONE',  ( 20.00000000000000000, -2.500000000000000444, -17.00000000000000000 ) ) ;
#8977 = CARTESIAN_POINT ( 'NONE',  ( 2.123976203522053741, -7.899625852120303549, 13.47898556379310087 ) ) ;
#8978 = CARTESIAN_POINT ( 'NONE',  ( 1.918921323896324083, 11.69058285425790977, 4.466082741316246718 ) ) ;
#8979 = CARTESIAN_POINT ( 'NONE',  ( 2.636624412715137922, 2.161493821597615828, 15.91454522070216093 ) ) ;
#8980 = CARTESIAN_POINT ( 'NONE',  ( 0.3151926232592501265, 13.09050869763092884, 4.172630140040843649 ) ) ;
#8981 = B_SPLINE_CURVE_WITH_KNOTS ( 'NONE', 3,
 ( #4979, #3638, #5163, #9472, #10919, #10816, #11193, #683, #2466, #8231, #8139, #14132, #18261 ),
 .UNSPECIFIED., .F., .F.,
 ( 4, 3, 3, 3, 4 ),
 ( 8.673617379884035472E-19, 0.0002299804304191491514, 0.0004599608082120254429, 0.0006467586077648011496, 0.0008336169836825998080 ),
 .UNSPECIFIED. ) ;
#8982 = CARTESIAN_POINT ( 'NONE',  ( 1.846138399168762101, 7.646096044339892650, 9.815003036200437236 ) ) ;
#8983 = ORIENTED_EDGE ( 'NONE', *, *, #8884, .F. ) ;
#8984 = VECTOR ( 'NONE', #17684, 1000.000000000000000 ) ;
#8985 = CARTESIAN_POINT ( 'NONE',  ( 2.636624412715137478, -2.862162146983530775, 15.80357026013314048 ) ) ;
#8987 = ORIENTED_EDGE ( 'NONE', *, *, #17186, .T. ) ;
#8986 = CARTESIAN_POINT ( 'NONE',  ( 3.950837973638676281, 12.81214529934975310, 6.888253895133341409 ) ) ;
#8988 = DIRECTION ( 'NONE',  ( 0.4246593920385850485, 0.1376957914266804250, -0.8948208031649687033 ) ) ;
#8989 = CARTESIAN_POINT ( 'NONE',  ( 16.56679352167444819, -0.004162264567718857756, 0.008311568981097966838 ) ) ;
#8990 = B_SPLINE_CURVE_WITH_KNOTS ( 'NONE', 3,
 ( #16168, #3052, #2124, #3547, #16466, #12063 ),
 .UNSPECIFIED., .F., .F.,
 ( 4, 2, 4 ),
 ( 0.000000000000000000, 0.001500839035891550705, 0.003001678071783101410 ),
 .UNSPECIFIED. ) ;
#8991 = ORIENTED_EDGE ( 'NONE', *, *, #2465, .T. ) ;
#8992 = CARTESIAN_POINT ( 'NONE',  ( 2.002547531651519996, -6.845637710436264456, 10.57595306287289638 ) ) ;
#8993 = UNCERTAINTY_MEASURE_WITH_UNIT (LENGTH_MEASURE( 1.000000000000000082E-05 ), #16404, 'distance_accuracy_value', 'NONE');
#8994 = DIRECTION ( 'NONE',  ( 0.000000000000000000, 1.000000000000000000, 0.000000000000000000 ) ) ;
#8995 = SHAPE_REPRESENTATION ( 'Central Pivot', ( #2030 ), #8722 ) ;
#8996 =( BOUNDED_SURFACE ( )  B_SPLINE_SURFACE ( 3, 1, ( 
 ( #6120, #17783 ),
 ( #3333, #3230 ),
 ( #9080, #9267 ),
 ( #15097, #1819 ) ),
 .UNSPECIFIED., .F., .F., .T. ) 
 B_SPLINE_SURFACE_WITH_KNOTS ( ( 4, 4 ),
 ( 2, 2 ),
 ( 0.000000000000000000, 1.000000000000000000 ),
 ( 0.000000000000000000, 1.000000000000000000 ),
 .UNSPECIFIED. ) 
 GEOMETRIC_REPRESENTATION_ITEM ( )  RATIONAL_B_SPLINE_SURFACE ( (
 ( 1.000000000000000000, 1.000000000000000000),
 ( 0.9933953342250436691, 0.8357391271907733676),
 ( 0.9933953342250436691, 0.8357391271907733676),
 ( 1.000000000000000000, 1.000000000000000000) ) ) 
 REPRESENTATION_ITEM ( '' )  SURFACE ( )  );
#8997 = ORIENTED_EDGE ( 'NONE', *, *, #14048, .F. ) ;
#8998 = VECTOR ( 'NONE', #355, 1000.000000000000000 ) ;
#8999 = EDGE_CURVE ( 'NONE', #12864, #3512, #16440, .T. ) ;
#9000 = CARTESIAN_POINT ( 'NONE',  ( 0.3148208552358917611, 13.73693263646118723, -0.2299193288887949882 ) ) ;
#9001 = CARTESIAN_POINT ( 'NONE',  ( 2.636624412714236865, 0.000000000000000000, 0.000000000000000000 ) ) ;
#9002 = CIRCLE ( 'NONE', #13587, 5.000000000000000000 ) ;
#9003 = CARTESIAN_POINT ( 'NONE',  ( 0.3307726912345216319, -13.74203354050372283, 0.5948952607472158816 ) ) ;
#9004 = ADVANCED_BREP_SHAPE_REPRESENTATION ( '', ( #10342, #2030 ), #13001 ) ;
#9005 = CIRCLE ( 'NONE', #16340, 16.06066017081991149 ) ;
#9006 = ORIENTED_EDGE ( 'NONE', *, *, #10230, .F. ) ;
#9007 = SHAPE_REPRESENTATION_RELATIONSHIP ( 'NONE' , 'NONE' ,  #13515, #9004 ) ;
#9008 = CARTESIAN_POINT ( 'NONE',  ( 2.636624412715435462, -15.80357026013316712, -2.862162146983298516 ) ) ;
#9009 = CARTESIAN_POINT ( 'NONE',  ( 20.00000000000000711, -24.99999999999999645, 6.000000000000000000 ) ) ;
#9010 = CARTESIAN_POINT ( 'NONE',  ( 16.56822296793089322, -0.003834730849370904075, 0.009385634690641608477 ) ) ;
#9011 = CARTESIAN_POINT ( 'NONE',  ( 0.4384471787762856398, 11.63197976518328680, 7.540925784514595165 ) ) ;
#9012 = CARTESIAN_POINT ( 'NONE',  ( 14.99999999999999289, 15.00000000000000000, 0.000000000000000000 ) ) ;
#9013 = VECTOR ( 'NONE', #2059, 1000.000000000000000 ) ;
#9014 = VERTEX_POINT ( 'NONE', #13134 ) ;
#9015 = DIRECTION ( 'NONE',  ( -1.000000000000000000, -0.000000000000000000, -0.000000000000000000 ) ) ;
#9016 = DIRECTION ( 'NONE',  ( 0.000000000000000000, 0.000000000000000000, -1.000000000000000000 ) ) ;
#9017 = AXIS2_PLACEMENT_3D ( 'NONE', #9636, #11178, #855 ) ;
#9018 = ORIENTED_EDGE ( 'NONE', *, *, #5973, .T. ) ;
#9019 = VERTEX_POINT ( 'NONE', #14188 ) ;
#9020 = CARTESIAN_POINT ( 'NONE',  ( 3.512766787570793969, 2.025881399556391127, 14.91422000116820179 ) ) ;
#9021 = ORIENTED_EDGE ( 'NONE', *, *, #7759, .F. ) ;
#9022 = CARTESIAN_POINT ( 'NONE',  ( 3.512766787570692273, -2.682019731918297012, -14.81029789862167867 ) ) ;
#9023 = ORIENTED_EDGE ( 'NONE', *, *, #18552, .F. ) ;
#9024 = EDGE_CURVE ( 'NONE', #12327, #8138, #501, .T. ) ;
#9025 = EDGE_CURVE ( 'NONE', #15958, #6394, #12754, .T. ) ;
#9026 = ADVANCED_FACE ( 'NONE', ( #11700 ), #11194, .T. ) ;
#9027 = CARTESIAN_POINT ( 'NONE',  ( 2.636624412714237309, 7.605649742761960042, 14.14563173255213613 ) ) ;
#9028 = CARTESIAN_POINT ( 'NONE',  ( 0.3150692679895994996, -13.73846569174796883, -0.1531143455845980217 ) ) ;
#9029 = CARTESIAN_POINT ( 'NONE',  ( 0.3170788640506440603, -0.1533108587037102788, 13.74111462631963576 ) ) ;
#9030 = CARTESIAN_POINT ( 'NONE',  ( 0.8740779401512095426, 7.708543377337996994, -12.04241618260087776 ) ) ;
#9031 = CIRCLE ( 'NONE', #11164, 16.06066017081991149 ) ;
#9032 = CARTESIAN_POINT ( 'NONE',  ( 0.4862570985993252548, 3.580942890621670482, 13.44146924561382583 ) ) ;
#9033 = FACE_OUTER_BOUND ( 'NONE', #13596, .T. ) ;
#9034 =( GEOMETRIC_REPRESENTATION_CONTEXT ( 3 ) GLOBAL_UNCERTAINTY_ASSIGNED_CONTEXT ( ( #1736 ) ) GLOBAL_UNIT_ASSIGNED_CONTEXT ( ( #1576, #1772, #11999 ) ) REPRESENTATION_CONTEXT ( 'NONE', 'WORKASPACE' ) );
#9035 = CARTESIAN_POINT ( 'NONE',  ( 1.254255976357524505, -1.011593778944422262, 14.64488542023450535 ) ) ;
#9036 = LINE ( 'NONE', #11709, #8187 ) ;
#9037 = DIRECTION ( 'NONE',  ( -0.000000000000000000, -0.000000000000000000, -1.000000000000000000 ) ) ;
#9038 = CARTESIAN_POINT ( 'NONE',  ( 0.3308579732646986238, -7.595989242675048381, -11.46737410776362509 ) ) ;
#9039 = DIRECTION ( 'NONE',  ( 0.000000000000000000, 1.000000000000000000, 0.000000000000000000 ) ) ;
#9040 = CARTESIAN_POINT ( 'NONE',  ( 1.562796894703937678, 1.635200584729765362E-15, 12.15840553252917289 ) ) ;
#9041 = ORIENTED_EDGE ( 'NONE', *, *, #17001, .F. ) ;
#9042 = VERTEX_POINT ( 'NONE', #15614 ) ;
#9043 = ORIENTED_EDGE ( 'NONE', *, *, #16867, .F. ) ;
#9044 = AXIS2_PLACEMENT_3D ( 'NONE', #16721, #14029, #15632 ) ;
#9045 = ORIENTED_EDGE ( 'NONE', *, *, #9217, .F. ) ;
#9046 = CARTESIAN_POINT ( 'NONE',  ( 0.3151928479966097374, 1.775918418904422640E-15, 13.73922861026898623 ) ) ;
#9047 = FACE_OUTER_BOUND ( 'NONE', #9994, .T. ) ;
#9048 = CARTESIAN_POINT ( 'NONE',  ( 1.847372867223026294, -12.44269075185938611, -0.1054171785007791406 ) ) ;
#9049 = CARTESIAN_POINT ( 'NONE',  ( 0.4862570985993235340, 13.89016912371017476, 0.7479633556562934604 ) ) ;
#9050 = CARTESIAN_POINT ( 'NONE',  ( 0.3307726912345205217, -11.46720933246392882, -7.596084275799019458 ) ) ;
#9051 = EDGE_CURVE ( 'NONE', #1583, #15356, #9945, .T. ) ;
#9052 = DIRECTION ( 'NONE',  ( 0.000000000000000000, 0.000000000000000000, 1.000000000000000000 ) ) ;
#9053 = CARTESIAN_POINT ( 'NONE',  ( 0.3095370825347234511, 13.20347358821919848, -3.806662003783274795 ) ) ;
#9054 = CARTESIAN_POINT ( 'NONE',  ( 1.847412631396503579, 12.44294644888238999, 0.04315047898439477309 ) ) ;
#9055 = AXIS2_PLACEMENT_3D ( 'NONE', #12006, #5604, #9137 ) ;
#9056 = DIRECTION ( 'NONE',  ( -1.000000000000000000, -0.000000000000000000, -0.000000000000000000 ) ) ;
#9057 = CARTESIAN_POINT ( 'NONE',  ( 0.000000000000000000, 1.805416924949539152E-15, 13.42403576283810906 ) ) ;
#9058 = CARTESIAN_POINT ( 'NONE',  ( 0.3151926232592488497, -11.16039997398647365, -8.013596737356504462 ) ) ;
#9059 = CARTESIAN_POINT ( 'NONE',  ( 0.000000000000000000, 0.000000000000000000, 0.000000000000000000 ) ) ;
#9060 = CARTESIAN_POINT ( 'NONE',  ( 0.3151928476913556376, 4.245457024760402653, -13.06684726503522320 ) ) ;
#9061 = AXIS2_PLACEMENT_3D ( 'NONE', #8837, #12092, #1868 ) ;
#9062 = EDGE_LOOP ( 'NONE', ( #3297, #18098, #11692, #1246 ) ) ;
#9063 = VERTEX_POINT ( 'NONE', #9878 ) ;
#9064 = VERTEX_POINT ( 'NONE', #2612 ) ;
#9065 = AXIS2_PLACEMENT_3D ( 'NONE', #16656, #3461, #10833 ) ;
#9066 = VERTEX_POINT ( 'NONE', #17243 ) ;
#9067 = LINE ( 'NONE', #2005, #4343 ) ;
#9068 = CIRCLE ( 'NONE', #829, 1.500000000000000000 ) ;
#9069 = DIRECTION ( 'NONE',  ( -1.000000000000000000, -0.000000000000000000, -0.000000000000000000 ) ) ;
#9070 = CARTESIAN_POINT ( 'NONE',  ( -32.49999999999999289, -12.50000000000000178, -7.071067811865460406 ) ) ;
#9071 = CLOSED_SHELL ( 'NONE', ( #1478, #17903, #1108, #9170, #8486, #16694, #8114, #6467, #5219, #7446, #14241, #15318 ) ) ;
#9072 = CARTESIAN_POINT ( 'NONE',  ( 3.950837973638676281, -10.05648675950133963, 10.51028938476214059 ) ) ;
#9073 = EDGE_CURVE ( 'NONE', #415, #209, #4159, .T. ) ;
#9074 = CARTESIAN_POINT ( 'NONE',  ( 3.074695600507584281, 13.70113613813179043, -7.366518011945612621 ) ) ;
#9075 = ORIENTED_EDGE ( 'NONE', *, *, #18497, .T. ) ;
#9076 = CARTESIAN_POINT ( 'NONE',  ( 2.816212223827430083, 7.499999999999999112, -15.81854889450411861 ) ) ;
#9077 = LINE ( 'NONE', #1817, #3784 ) ;
#9078 = EDGE_CURVE ( 'NONE', #11185, #182, #8925, .T. ) ;
#9079 = DIRECTION ( 'NONE',  ( 0.000000000000000000, -1.000000000000000000, 0.000000000000000000 ) ) ;
#9080 = CARTESIAN_POINT ( 'NONE',  ( 16.56822296793089322, -0.009385634690642031749, 0.003834730849371980905 ) ) ;
#9081 =( BOUNDED_SURFACE ( )  B_SPLINE_SURFACE ( 3, 1, ( 
 ( #3186, #248 ),
 ( #13140, #5771 ),
 ( #17447, #11710 ),
 ( #149, #1673 ) ),
 .UNSPECIFIED., .F., .F., .T. ) 
 B_SPLINE_SURFACE_WITH_KNOTS ( ( 4, 4 ),
 ( 2, 2 ),
 ( 0.000000000000000000, 1.000000000000000000 ),
 ( 0.000000000000000000, 1.000000000000000000 ),
 .UNSPECIFIED. ) 
 GEOMETRIC_REPRESENTATION_ITEM ( )  RATIONAL_B_SPLINE_SURFACE ( (
 ( 1.000000000000000000, 1.000000000000000000),
 ( 0.7792777138730158093, 0.9689936506012928330),
 ( 0.7792777138730158093, 0.9689936506012928330),
 ( 1.000000000000000000, 1.000000000000000000) ) ) 
 REPRESENTATION_ITEM ( '' )  SURFACE ( )  );
#9082 = CARTESIAN_POINT ( 'NONE',  ( 0.4862570985993252548, 3.580942890621670482, 13.44146924561382583 ) ) ;
#9083 = CARTESIAN_POINT ( 'NONE',  ( 8.522092701127531811, -6.946128462138598358, 0.3779863304870977325 ) ) ;
#9084 = CARTESIAN_POINT ( 'NONE',  ( 0.3095370825347224519, -4.681152801286072140, -12.91933430393612703 ) ) ;
#9085 = ORIENTED_EDGE ( 'NONE', *, *, #6224, .T. ) ;
#9086 = CARTESIAN_POINT ( 'NONE',  ( 1.977436885025421809, 14.12046670317507058, 6.153171729167918436 ) ) ;
#9088 = ORIENTED_EDGE ( 'NONE', *, *, #17310, .T. ) ;
#9087 = DIRECTION ( 'NONE',  ( 0.000000000000000000, 0.000000000000000000, 1.000000000000000000 ) ) ;
#9089 = CARTESIAN_POINT ( 'NONE',  ( 1.560000000000000053, -0.8660254037844384856, -1.500000000000000000 ) ) ;
#9090 = ORIENTED_EDGE ( 'NONE', *, *, #7311, .F. ) ;
#9091 = ADVANCED_FACE ( 'NONE', ( #7706 ), #7980, .F. ) ;
#9092 = DIRECTION ( 'NONE',  ( 0.000000000000000000, 0.000000000000000000, -1.000000000000000000 ) ) ;
#9093 = VECTOR ( 'NONE', #11157, 1000.000000000000227 ) ;
#9094 = ORIENTED_EDGE ( 'NONE', *, *, #10451, .F. ) ;
#9095 = CARTESIAN_POINT ( 'NONE',  ( 0.3137051932979792457, -12.91601973349266963, -4.679953077377624560 ) ) ;
#9096 = CARTESIAN_POINT ( 'NONE',  ( 6.538348415311011408, -2.499999999999998668, -12.00000000000000000 ) ) ;
#9097 = ORIENTED_EDGE ( 'NONE', *, *, #7745, .T. ) ;
#9098 = CARTESIAN_POINT ( 'NONE',  ( 16.57778382496167424, -0.01092721432668986720, -0.01018821665058789253 ) ) ;
#9099 = CARTESIAN_POINT ( 'NONE',  ( 0.3720661004400040439, 13.79610186261029980, -0.7231997263365288475 ) ) ;
#9100 = DIRECTION ( 'NONE',  ( -1.000000000000000000, 0.000000000000000000, 0.000000000000000000 ) ) ;
#9101 = CARTESIAN_POINT ( 'NONE',  ( 0.8740764193768466583, -11.05257066464528748, -9.070946295054149289 ) ) ;
#9102 = ORIENTED_EDGE ( 'NONE', *, *, #9332, .F. ) ;
#9103 = ADVANCED_FACE ( 'NONE', ( #8836 ), #1963, .F. ) ;
#9104 = VECTOR ( 'NONE', #412, 1000.000000000000000 ) ;
#9105 =( NAMED_UNIT ( * ) PLANE_ANGLE_UNIT ( ) SI_UNIT ( $, .RADIAN. ) );
#9106 = CARTESIAN_POINT ( 'NONE',  ( 16.57778382496167424, -0.01018821665058842162, -0.01092721432669105028 ) ) ;
#9107 = CARTESIAN_POINT ( 'NONE',  ( 11.50000000000000178, 0.000000000000000000, 10.00000000000000000 ) ) ;
#9108 = DIRECTION ( 'NONE',  ( 0.000000000000000000, 0.000000000000000000, -1.000000000000000000 ) ) ;
#9110 = VERTEX_POINT ( 'NONE', #11994 ) ;
#9109 = DIRECTION ( 'NONE',  ( -0.000000000000000000, 0.000000000000000000, 1.000000000000000000 ) ) ;
#9111 = B_SPLINE_CURVE_WITH_KNOTS ( 'NONE', 3,
 ( #11942, #3125, #3325, #10316, #8971, #14801 ),
 .UNSPECIFIED., .F., .F.,
 ( 4, 2, 4 ),
 ( 4.878909776184769953E-19, 0.001657017934711441055, 0.003314035869422881676 ),
 .UNSPECIFIED. ) ;
#9112 = EDGE_CURVE ( 'NONE', #10941, #10024, #17788, .T. ) ;
#9113 = SHAPE_REPRESENTATION ( 'Handle Arm 1', ( #2030 ), #1089 ) ;
#9114 = VERTEX_POINT ( 'NONE', #4542 ) ;
#9115 = CARTESIAN_POINT ( 'NONE',  ( 0.3137051932979757485, 12.91601973349276733, -4.679953077377353665 ) ) ;
#9116 =( BOUNDED_SURFACE ( )  B_SPLINE_SURFACE ( 3, 1, ( 
 ( #12455, #16946 ),
 ( #11033, #16849 ),
 ( #9581, #15413 ),
 ( #2320, #8167 ) ),
 .UNSPECIFIED., .F., .F., .T. ) 
 B_SPLINE_SURFACE_WITH_KNOTS ( ( 4, 4 ),
 ( 2, 2 ),
 ( 0.000000000000000000, 1.000000000000000000 ),
 ( 0.000000000000000000, 1.000000000000000000 ),
 .UNSPECIFIED. ) 
 GEOMETRIC_REPRESENTATION_ITEM ( )  RATIONAL_B_SPLINE_SURFACE ( (
 ( 1.000000000000000000, 1.000000000000000000),
 ( 0.7792777138730158093, 0.9689936506012928330),
 ( 0.7792777138730158093, 0.9689936506012928330),
 ( 1.000000000000000000, 1.000000000000000000) ) ) 
 REPRESENTATION_ITEM ( '' )  SURFACE ( )  );
#9117 = CARTESIAN_POINT ( 'NONE',  ( 0.3939875929385656117, -13.80036004410495210, 0.7003304234512695015 ) ) ;
#9118 = ORIENTED_EDGE ( 'NONE', *, *, #15368, .F. ) ;
#9119 = ORIENTED_EDGE ( 'NONE', *, *, #3071, .T. ) ;
#9120 = CARTESIAN_POINT ( 'NONE',  ( 0.4862570985993235340, -8.769551628660812170, 10.79774104611370333 ) ) ;
#9121 = VERTEX_POINT ( 'NONE', #17828 ) ;
#9122 = DIRECTION ( 'NONE',  ( -0.000000000000000000, -0.000000000000000000, -1.000000000000000000 ) ) ;
#9123 = ORIENTED_EDGE ( 'NONE', *, *, #5834, .F. ) ;
#9124 = DIRECTION ( 'NONE',  ( -1.000000000000000000, 0.000000000000000000, 0.000000000000000000 ) ) ;
#9125 = LINE ( 'NONE', #10267, #14531 ) ;
#9126 = LINE ( 'NONE', #7611, #17612 ) ;
#9127 = CARTESIAN_POINT ( 'NONE',  ( 16.57605080000000086, 6.799999999999999822, 1.500000000000000000 ) ) ;
#9128 = CARTESIAN_POINT ( 'NONE',  ( 3.950837973638668288, 0.000000000000000000, 0.000000000000000000 ) ) ;
#9129 = CARTESIAN_POINT ( 'NONE',  ( 2.747332970342022840, -7.289199830147006232, -14.63517873738954655 ) ) ;
#9130 = DIRECTION ( 'NONE',  ( -0.000000000000000000, -0.000000000000000000, 1.000000000000000000 ) ) ;
#9131 = DIRECTION ( 'NONE',  ( 0.7561779333270775005, 0.5081796452863215352, 0.4122479608995760492 ) ) ;
#9132 = CARTESIAN_POINT ( 'NONE',  ( 1.321128355694181398E-14, -9.013167318348349610, 33.78111653772642597 ) ) ;
#9133 = EDGE_CURVE ( 'NONE', #10024, #17449, #13445, .T. ) ;
#9134 = EDGE_CURVE ( 'NONE', #8612, #17983, #4100, .T. ) ;
#9135 = EDGE_CURVE ( 'NONE', #17750, #16605, #14658, .T. ) ;
#9136 = CARTESIAN_POINT ( 'NONE',  ( 1.846613052777650310, -11.93415846513959444, -3.520031056876430142 ) ) ;
#9137 = DIRECTION ( 'NONE',  ( 0.000000000000000000, 0.000000000000000000, 1.000000000000000000 ) ) ;
#9138 = CIRCLE ( 'NONE', #14927, 16.06066017081991149 ) ;
#9139 = VERTEX_POINT ( 'NONE', #4831 ) ;
#9140 = VERTEX_POINT ( 'NONE', #13512 ) ;
#9141 = VERTEX_POINT ( 'NONE', #16397 ) ;
#9142 = ORIENTED_EDGE ( 'NONE', *, *, #4690, .T. ) ;
#9143 = VECTOR ( 'NONE', #753, 1000.000000000000000 ) ;
#9144 = CARTESIAN_POINT ( 'NONE',  ( 1.846138399168762101, -11.95493567637852905, 3.446241763652952539 ) ) ;
#9145 = DIRECTION ( 'NONE',  ( 0.000000000000000000, 0.000000000000000000, -1.000000000000000000 ) ) ;
#9146 = EDGE_CURVE ( 'NONE', #204, #14986, #9125, .T. ) ;
#9147 = CARTESIAN_POINT ( 'NONE',  ( 16.56753206892534891, 0.008490833999798923920, 0.004253784598196209618 ) ) ;
#9148 = DIRECTION ( 'NONE',  ( -1.000000000000000000, -0.000000000000000000, -0.000000000000000000 ) ) ;
#9149 = CARTESIAN_POINT ( 'NONE',  ( 3.512766787570690497, 2.682019731918607430, -14.81029789862162893 ) ) ;
#9150 = DIRECTION ( 'NONE',  ( -1.000000000000000000, 0.000000000000000000, 0.000000000000000000 ) ) ;
#9151 = CARTESIAN_POINT ( 'NONE',  ( 0.3148213771069364175, 7.888490156175222090, 11.24846294176314387 ) ) ;
#9152 = CARTESIAN_POINT ( 'NONE',  ( 1.846613052777651420, 11.72395935470504291, -4.166957398589727468 ) ) ;
#9153 = CARTESIAN_POINT ( 'NONE',  ( 0.3137051932979809665, 13.20008686438111312, -3.805684345189650042 ) ) ;
#9154 = CARTESIAN_POINT ( 'NONE',  ( 1.846138399168762101, -7.646096044339961040, 9.815003036200383946 ) ) ;
#9155 = DIRECTION ( 'NONE',  ( 1.000000000000000000, 0.000000000000000000, 0.000000000000000000 ) ) ;
#9156 = CARTESIAN_POINT ( 'NONE',  ( 0.3150686449036048109, 4.099563462784836965, -13.11344473514184372 ) ) ;
#9157 = ORIENTED_EDGE ( 'NONE', *, *, #16964, .F. ) ;
#9158 = ORIENTED_EDGE ( 'NONE', *, *, #3114, .T. ) ;
#9159 = ADVANCED_FACE ( 'NONE', ( #3077 ), #2797, .F. ) ;
#9160 = ORIENTED_EDGE ( 'NONE', *, *, #8507, .T. ) ;
#9161 = ADVANCED_FACE ( 'NONE', ( #3279 ), #239, .T. ) ;
#9162 = ORIENTED_EDGE ( 'NONE', *, *, #10230, .T. ) ;
#9163 = CARTESIAN_POINT ( 'NONE',  ( 3.512766787570702043, -7.127386085302744867, -13.25664064834487021 ) ) ;
#9164 = CARTESIAN_POINT ( 'NONE',  ( 2.636624412715435462, -15.80357026013316712, -2.862162146983298516 ) ) ;
#9165 = CARTESIAN_POINT ( 'NONE',  ( 0.3095370825347224519, -12.91933430393604709, -4.681152801286295073 ) ) ;
#9166 = CARTESIAN_POINT ( 'NONE',  ( 0.4862570985993235340, -13.44146924561383827, 3.580942890621619412 ) ) ;
#9167 = CARTESIAN_POINT ( 'NONE',  ( 1.254009781011571567, 1.011465182608068503, 14.64464726212582590 ) ) ;
#9168 = ORIENTED_EDGE ( 'NONE', *, *, #8643, .T. ) ;
#9169 = CARTESIAN_POINT ( 'NONE',  ( 4.160991745704745171, 7.500000000000000888, -16.52287405655582475 ) ) ;
#9170 = ADVANCED_FACE ( 'NONE', ( #4637 ), #14949, .T. ) ;
#9171 = CARTESIAN_POINT ( 'NONE',  ( 0.3720661004400037664, -3.575426119359092159, -13.34435358167256247 ) ) ;
#9172 = FACE_OUTER_BOUND ( 'NONE', #230, .T. ) ;
#9173 = CARTESIAN_POINT ( 'NONE',  ( 16.58200780006414732, 0.007066318000004704822, 0.008650561019685554590 ) ) ;
#9174 = CARTESIAN_POINT ( 'NONE',  ( 3.950837973638676281, 10.05648675950141602, -10.51028938476206953 ) ) ;
#9175 = CARTESIAN_POINT ( 'NONE',  ( 1.845756295923360657, -6.920504327368265152, 10.33914852636102033 ) ) ;
#9176 = AXIS2_PLACEMENT_3D ( 'NONE', #10751, #429, #11993 ) ;
#9177 = ORIENTED_EDGE ( 'NONE', *, *, #17597, .F. ) ;
#9178 = FACE_OUTER_BOUND ( 'NONE', #8375, .T. ) ;
#9180 = ORIENTED_EDGE ( 'NONE', *, *, #12708, .T. ) ;
#9179 = CARTESIAN_POINT ( 'NONE',  ( 16.56679352167444819, -0.006526964904753006572, -0.006618561353599182288 ) ) ;
#9181 = LINE ( 'NONE', #16734, #2338 ) ;
#9182 = EDGE_CURVE ( 'NONE', #17372, #12766, #16980, .T. ) ;
#9183 = DIRECTION ( 'NONE',  ( 1.000000000000000000, 0.000000000000000000, 0.000000000000000000 ) ) ;
#9184 = EDGE_LOOP ( 'NONE', ( #13871, #12656, #10965, #16752 ) ) ;
#9185 = CARTESIAN_POINT ( 'NONE',  ( 0.4862570985993235340, -0.7479633556561480212, -13.89016912371018186 ) ) ;
#9186 = CARTESIAN_POINT ( 'NONE',  ( -0.9342146476564506807, -7.500000000000132339, -13.05973490260134362 ) ) ;
#9187 = ADVANCED_FACE ( 'NONE', ( #3852 ), #18291, .T. ) ;
#9188 =( BOUNDED_SURFACE ( )  B_SPLINE_SURFACE ( 3, 1, ( 
 ( #5615, #6985 ),
 ( #11468, #14606 ),
 ( #15856, #16042 ),
 ( #4205, #12797 ) ),
 .UNSPECIFIED., .F., .F., .T. ) 
 B_SPLINE_SURFACE_WITH_KNOTS ( ( 4, 4 ),
 ( 2, 2 ),
 ( 0.000000000000000000, 1.000000000000000000 ),
 ( 0.000000000000000000, 1.000000000000000000 ),
 .UNSPECIFIED. ) 
 GEOMETRIC_REPRESENTATION_ITEM ( )  RATIONAL_B_SPLINE_SURFACE ( (
 ( 1.000000000000000000, 1.000000000000000000),
 ( 0.7792777138730160313, 0.9689936506012927220),
 ( 0.7792777138730160313, 0.9689936506012927220),
 ( 1.000000000000000000, 1.000000000000000000) ) ) 
 REPRESENTATION_ITEM ( '' )  SURFACE ( )  );
#9189 = VERTEX_POINT ( 'NONE', #15324 ) ;
#9190 = CARTESIAN_POINT ( 'NONE',  ( 16.58200780006414732, -0.004047297414157817463, -0.01041078477703986926 ) ) ;
#9191 = CARTESIAN_POINT ( 'NONE',  ( 0.3137051932979792457, -10.83767969834796929, -8.442169467526971616 ) ) ;
#9192 = CARTESIAN_POINT ( 'NONE',  ( 16.56679352167444819, -0.006526964904753006572, -0.006618561353599182288 ) ) ;
#9193 = CARTESIAN_POINT ( 'NONE',  ( 0.3137051932979809665, 3.805684345189785933, 13.20008686438107581 ) ) ;
#9194 = B_SPLINE_CURVE_WITH_KNOTS ( 'NONE', 3,
 ( #16633, #588, #9637, #15467, #9466, #2198 ),
 .UNSPECIFIED., .F., .F.,
 ( 4, 2, 4 ),
 ( 0.000000000000000000, 0.001656992708824380845, 0.003313985417648761689 ),
 .UNSPECIFIED. ) ;
#9195 = EDGE_CURVE ( 'NONE', #8605, #16257, #13985, .T. ) ;
#9196 = CIRCLE ( 'NONE', #14989, 10.00000000000000888 ) ;
#9197 = CARTESIAN_POINT ( 'NONE',  ( 1.918918678667044908, -6.832809802519085096, 10.48466773720559608 ) ) ;
#9198 = LINE ( 'NONE', #317, #17338 ) ;
#9199 = FACE_OUTER_BOUND ( 'NONE', #18790, .T. ) ;
#9201 = VERTEX_POINT ( 'NONE', #628 ) ;
#9200 = CARTESIAN_POINT ( 'NONE',  ( 16.56753206892534891, 0.001421777558675947238, -0.009389754735542250527 ) ) ;
#9202 = CARTESIAN_POINT ( 'NONE',  ( -4.000000000000000888, 17.00000000000000000, 7.000000000000000000 ) ) ;
#9203 = VERTEX_POINT ( 'NONE', #18106 ) ;
#9204 = CARTESIAN_POINT ( 'NONE',  ( 0.4754618798421171855, -7.564402563418553882, 11.68486377711963797 ) ) ;
#9205 = CARTESIAN_POINT ( 'NONE',  ( 2.002547531651519996, 11.75462648437108015, -4.532360870844206246 ) ) ;
#9206 = ORIENTED_EDGE ( 'NONE', *, *, #2727, .T. ) ;
#9207 = ORIENTED_EDGE ( 'NONE', *, *, #13647, .F. ) ;
#9209 = CARTESIAN_POINT ( 'NONE',  ( 2.750000000000000000, 0.000000000000000000, 0.000000000000000000 ) ) ;
#9208 = AXIS2_PLACEMENT_3D ( 'NONE', #13869, #18000, #10644 ) ;
#9210 = ORIENTED_EDGE ( 'NONE', *, *, #11124, .T. ) ;
#9211 = CARTESIAN_POINT ( 'NONE',  ( 3.074695600508143833, 13.70113613813285269, 7.366518011945069055 ) ) ;
#9212 = VERTEX_POINT ( 'NONE', #4922 ) ;
#9213 = EDGE_CURVE ( 'NONE', #4747, #17792, #13585, .T. ) ;
#9214 = CARTESIAN_POINT ( 'NONE',  ( 0.4754618798421162973, -13.89949764182683190, 0.7484603771383941950 ) ) ;
#9215 = DIRECTION ( 'NONE',  ( 0.7635533937278216055, 0.02138673900302332995, -0.6453904417649386493 ) ) ;
#9216 = DIRECTION ( 'NONE',  ( -0.000000000000000000, 1.000000000000000000, -0.000000000000000000 ) ) ;
#9217 = EDGE_CURVE ( 'NONE', #8021, #1012, #7536, .T. ) ;
#9218 = PRODUCT_DEFINITION_SHAPE ( 'NONE', 'NONE',  #18911 ) ;
#9219 = CARTESIAN_POINT ( 'NONE',  ( 3.512766787570770433, -2.025881399556492823, 14.91422000116819113 ) ) ;
#9220 = CARTESIAN_POINT ( 'NONE',  ( 0.4754618798421167414, 5.007009103465430044, -12.98792082933639058 ) ) ;
#9221 = CARTESIAN_POINT ( 'NONE',  ( 15.00000000000000711, -45.00000000000000000, 3.000000000000000000 ) ) ;
#9222 = B_SPLINE_CURVE_WITH_KNOTS ( 'NONE', 3,
 ( #3065, #418, #16484, #4622, #3367, #12081, #18005, #13211, #8912, #10550, #17913, #14739, #7495 ),
 .UNSPECIFIED., .F., .F.,
 ( 4, 3, 3, 3, 4 ),
 ( 3.878959614448864246E-18, 0.0002299780670421047908, 0.0004599561239687891445, 0.0006896788984287886056, 0.0009194956271626397379 ),
 .UNSPECIFIED. ) ;
#9223 = CARTESIAN_POINT ( 'NONE',  ( 1.562796894703937678, 0.000000000000000000, 0.000000000000000000 ) ) ;
#9224 =( BOUNDED_SURFACE ( )  B_SPLINE_SURFACE ( 3, 1, ( 
 ( #4770, #10404 ),
 ( #477, #11844 ),
 ( #4867, #10700 ),
 ( #7653, #5902 ) ),
 .UNSPECIFIED., .F., .F., .F. ) 
 B_SPLINE_SURFACE_WITH_KNOTS ( ( 4, 4 ),
 ( 2, 2 ),
 ( 0.000000000000000000, 1.000000000000000000 ),
 ( 0.000000000000000000, 1.000000000000000000 ),
 .UNSPECIFIED. ) 
 GEOMETRIC_REPRESENTATION_ITEM ( )  RATIONAL_B_SPLINE_SURFACE ( (
 ( 1.000000000000000000, 1.000000000000000000),
 ( 0.9933953342250436691, 0.8357391271907733676),
 ( 0.9933953342250436691, 0.8357391271907733676),
 ( 1.000000000000000000, 1.000000000000000000) ) ) 
 REPRESENTATION_ITEM ( '' )  SURFACE ( )  );
#9225 = CARTESIAN_POINT ( 'NONE',  ( 1.847168016377982669, 7.161712042621604546, -10.17509564929251020 ) ) ;
#9226 = CARTESIAN_POINT ( 'NONE',  ( 2.002547531651519996, 12.57989064830759496, -0.6781519942172177240 ) ) ;
#9227 = LINE ( 'NONE', #17645, #10926 ) ;
#9228 = VECTOR ( 'NONE', #15478, 1000.000000000000000 ) ;
#9229 = FILL_AREA_STYLE ('',( #10671 ) ) ;
#9230 = EDGE_LOOP ( 'NONE', ( #8, #17889, #4039, #16889 ) ) ;
#9231 = ORIENTED_EDGE ( 'NONE', *, *, #16587, .T. ) ;
#9232 = ORIENTED_EDGE ( 'NONE', *, *, #15792, .F. ) ;
#9233 = VERTEX_POINT ( 'NONE', #6644 ) ;
#9234 = DIRECTION ( 'NONE',  ( -0.000000000000000000, -0.000000000000000000, 1.000000000000000000 ) ) ;
#9235 = DIRECTION ( 'NONE',  ( -1.913297951445007868E-16, 1.000000000000000000, 0.000000000000000000 ) ) ;
#9236 = CARTESIAN_POINT ( 'NONE',  ( 2.697797270744668463, -12.33058466479264936, -4.970631985779717432 ) ) ;
#9237 = CARTESIAN_POINT ( 'NONE',  ( -110.4113270445337918, -81.60345299795268659, -91.28051051278382033 ) ) ;
#9238 = EDGE_CURVE ( 'NONE', #2882, #9233, #5945, .T. ) ;
#9239 = EDGE_CURVE ( 'NONE', #16984, #6765, #18220, .T. ) ;
#9240 = CARTESIAN_POINT ( 'NONE',  ( -30.00000000000000355, -12.50000000000000178, 3.000000000000000000 ) ) ;
#9241 = EDGE_CURVE ( 'NONE', #9042, #14205, #17245, .T. ) ;
#9242 = PRODUCT_DEFINITION_CONTEXT ( 'detailed design', #3386, 'design' ) ;
#9243 = DIRECTION ( 'NONE',  ( 1.000000000000000000, 0.000000000000000000, 0.000000000000000000 ) ) ;
#9244 = DIRECTION ( 'NONE',  ( 0.000000000000000000, 0.000000000000000000, 1.000000000000000000 ) ) ;
#9245 = CARTESIAN_POINT ( 'NONE',  ( 16.56753206892534891, 0.001421777558675943985, -0.009389754735542252262 ) ) ;
#9246 = CARTESIAN_POINT ( 'NONE',  ( 0.3137051932979809665, 10.83767969834803324, 8.442169467526891680 ) ) ;
#9247 = CARTESIAN_POINT ( 'NONE',  ( 8.522092701127531811, -0.3779863304870734741, -6.946128462138600135 ) ) ;
#9248 = FACE_OUTER_BOUND ( 'NONE', #18172, .T. ) ;
#9249 = CIRCLE ( 'NONE', #6513, 5.000000000000000000 ) ;
#9250 = ORIENTED_EDGE ( 'NONE', *, *, #8589, .F. ) ;
#9251 = EDGE_LOOP ( 'NONE', ( #8609, #7114 ) ) ;
#9252 = VERTEX_POINT ( 'NONE', #6546 ) ;
#9253 = EDGE_LOOP ( 'NONE', ( #10673, #14817, #4844, #7561 ) ) ;
#9254 = CARTESIAN_POINT ( 'NONE',  ( 1.847380140988736708, -7.402792205949027426, -10.00162556679659076 ) ) ;
#9255 = LINE ( 'NONE', #4677, #6864 ) ;
#9256 = DIRECTION ( 'NONE',  ( 0.000000000000000000, 0.000000000000000000, 1.000000000000000000 ) ) ;
#9257 = CARTESIAN_POINT ( 'NONE',  ( 2.426025403784448642, 0.000000000000000000, 2.168404344971008868E-16 ) ) ;
#9258 = CARTESIAN_POINT ( 'NONE',  ( 22.30499999999999972, 0.000000000000000000, 2.500000000000000888 ) ) ;
#9259 = ORIENTED_EDGE ( 'NONE', *, *, #11552, .T. ) ;
#9260 = EDGE_CURVE ( 'NONE', #15610, #11688, #10852, .T. ) ;
#9261 = CARTESIAN_POINT ( 'NONE',  ( 0.4862570985993235340, 3.580942890621860109, -13.44146924561377254 ) ) ;
#9262 = CIRCLE ( 'NONE', #11697, 2.700000000000000178 ) ;
#9263 = EDGE_CURVE ( 'NONE', #5420, #7234, #15237, .T. ) ;
#9264 = CARTESIAN_POINT ( 'NONE',  ( 0.3148208552358988666, 13.13564827777588917, 4.026279359288469806 ) ) ;
#9265 = EDGE_CURVE ( 'NONE', #15782, #3563, #18770, .T. ) ;
#9266 = CARTESIAN_POINT ( 'NONE',  ( -2.117882332753601826, 7.499999999999999112, -15.34025089741873238 ) ) ;
#9267 = CARTESIAN_POINT ( 'NONE',  ( 0.3720661004400037664, 12.89739157014192550, 4.951033743989683877 ) ) ;
#9268 = EDGE_CURVE ( 'NONE', #4825, #14717, #9411, .T. ) ;
#9269 = CARTESIAN_POINT ( 'NONE',  ( 0.4862570985993235340, 8.769551628660890330, -10.79774104611363761 ) ) ;
#9270 = CARTESIAN_POINT ( 'NONE',  ( 0.3151928479966097374, 0.000000000000000000, -13.73922861026898623 ) ) ;
#9271 = ORIENTED_EDGE ( 'NONE', *, *, #4630, .F. ) ;
#9272 = CARTESIAN_POINT ( 'NONE',  ( 0.4754618798421167414, -3.583352865732579051, -13.45049478164063217 ) ) ;
#9274 = ORIENTED_EDGE ( 'NONE', *, *, #17142, .F. ) ;
#9273 = CARTESIAN_POINT ( 'NONE',  ( 16.57605080000000086, 6.799999999999999822, -1.500000000000000000 ) ) ;
#9275 = CARTESIAN_POINT ( 'NONE',  ( 3.950837973638675393, -10.51028938476224894, 10.05648675950122595 ) ) ;
#9276 = VECTOR ( 'NONE', #15516, 1000.000000000000000 ) ;
#9277 = VECTOR ( 'NONE', #11631, 1000.000000000000000 ) ;
#9278 = CARTESIAN_POINT ( 'NONE',  ( 0.4862570985993235340, 10.79774104611385965, -8.769551628660616771 ) ) ;
#9279 = ORIENTED_EDGE ( 'NONE', *, *, #13726, .F. ) ;
#9280 = DIRECTION ( 'NONE',  ( 0.000000000000000000, 0.000000000000000000, -1.000000000000000000 ) ) ;
#9281 = CARTESIAN_POINT ( 'NONE',  ( -2.817269318714846094, -7.500000000000000888, -15.81922481682703996 ) ) ;
#9282 = ORIENTED_EDGE ( 'NONE', *, *, #18077, .F. ) ;
#9283 = LINE ( 'NONE', #2032, #6938 ) ;
#9284 = CARTESIAN_POINT ( 'NONE',  ( 0.3151928476913591903, 13.73922860838471749, -0.0002082997484259338093 ) ) ;
#9285 = CARTESIAN_POINT ( 'NONE',  ( 0.3132635586635981184, -8.495712071659319520, -10.79541209008113256 ) ) ;
#9286 = CARTESIAN_POINT ( 'NONE',  ( 1.847247051441589960, 10.16425585218611083, -7.177495230324590025 ) ) ;
#9287 = EDGE_CURVE ( 'NONE', #347, #2337, #2300, .T. ) ;
#9288 = AXIS2_PLACEMENT_3D ( 'NONE', #13021, #1180, #3958 ) ;
#9289 = EDGE_CURVE ( 'NONE', #13349, #14649, #6735, .T. ) ;
#9290 = PRODUCT_DEFINITION_FORMATION_WITH_SPECIFIED_SOURCE ( 'ANY', '', #4477, .NOT_KNOWN. ) ;
#9291 =( NAMED_UNIT ( * ) SI_UNIT ( $, .STERADIAN. ) SOLID_ANGLE_UNIT ( ) );
#9292 = DIRECTION ( 'NONE',  ( -1.000000000000000000, -1.734723475976807094E-16, 0.000000000000000000 ) ) ;
#9293 = ORIENTED_EDGE ( 'NONE', *, *, #14599, .T. ) ;
#9294 = DIRECTION ( 'NONE',  ( -1.000000000000000000, 0.000000000000000000, 0.000000000000000000 ) ) ;
#9296 = VERTEX_POINT ( 'NONE', #7902 ) ;
#9295 = CARTESIAN_POINT ( 'NONE',  ( 0.4754618798421162973, -0.7484603771383456783, -13.89949764182683545 ) ) ;
#9297 = CARTESIAN_POINT ( 'NONE',  ( 1.342453679581834924, -11.38190519890846453, -9.456403821038923851 ) ) ;
#9298 = CARTESIAN_POINT ( 'NONE',  ( 0.4754618798421162973, 3.583352865732667425, 13.45049478164061441 ) ) ;
#9299 = CARTESIAN_POINT ( 'NONE',  ( 3.950837973638676281, 13.10350451991840615, 6.316429227969512894 ) ) ;
#9300 = FACE_OUTER_BOUND ( 'NONE', #7159, .T. ) ;
#9301 =( BOUNDED_SURFACE ( )  B_SPLINE_SURFACE ( 3, 1, ( 
 ( #11441, #14393 ),
 ( #1300, #14582 ),
 ( #1500, #1400 ),
 ( #2811, #8763 ) ),
 .UNSPECIFIED., .F., .F., .T. ) 
 B_SPLINE_SURFACE_WITH_KNOTS ( ( 4, 4 ),
 ( 2, 2 ),
 ( 0.000000000000000000, 1.000000000000000000 ),
 ( 0.000000000000000000, 1.000000000000000000 ),
 .UNSPECIFIED. ) 
 GEOMETRIC_REPRESENTATION_ITEM ( )  RATIONAL_B_SPLINE_SURFACE ( (
 ( 1.000000000000000000, 1.000000000000000000),
 ( 0.9593108457356467333, 0.9995965569486454649),
 ( 0.9593108457356467333, 0.9995965569486454649),
 ( 1.000000000000000000, 1.000000000000000000) ) ) 
 REPRESENTATION_ITEM ( '' )  SURFACE ( )  );
#9302 = ORIENTED_EDGE ( 'NONE', *, *, #3221, .T. ) ;
#9303 = VECTOR ( 'NONE', #2748, 1000.000000000000000 ) ;
#9304 = EDGE_LOOP ( 'NONE', ( #551, #11456, #12534, #14043, #2449 ) ) ;
#9305 = CARTESIAN_POINT ( 'NONE',  ( 0.3151926232592440202, 11.07013665200807395, -8.137833541809259330 ) ) ;
#9306 = EDGE_CURVE ( 'NONE', #14151, #15676, #11150, .T. ) ;
#9307 = ORIENTED_EDGE ( 'NONE', *, *, #6340, .T. ) ;
#9308 = DIRECTION ( 'NONE',  ( 0.000000000000000000, 0.000000000000000000, 1.000000000000000000 ) ) ;
#9309 = ORIENTED_EDGE ( 'NONE', *, *, #4609, .F. ) ;
#9310 = AXIS2_PLACEMENT_3D ( 'NONE', #8894, #17603, #16268 ) ;
#9311 = LINE ( 'NONE', #15143, #6411 ) ;
#9312 = PRODUCT_RELATED_PRODUCT_CATEGORY ( 'part', '', ( #10755 ) ) ;
#9313 = CARTESIAN_POINT ( 'NONE',  ( 7.000000000000000000, 8.572527594031473190E-16, 3.000000000000000000 ) ) ;
#9314 = ADVANCED_FACE ( 'NONE', ( #12276 ), #14446, .T. ) ;
#9315 = CARTESIAN_POINT ( 'NONE',  ( -194.9999999999999716, -10.00000000000002665, 6.000000000000000000 ) ) ;
#9316 = DIRECTION ( 'NONE',  ( 0.000000000000000000, 0.000000000000000000, 1.000000000000000000 ) ) ;
#9317 = EDGE_CURVE ( 'NONE', #2137, #9780, #5041, .T. ) ;
#9318 = CARTESIAN_POINT ( 'NONE',  ( 0.4862570985993252548, 12.97920246947879441, 5.003653737315533867 ) ) ;
#9319 = CARTESIAN_POINT ( 'NONE',  ( 2.002547531651519996, -0.6781519942170860515, -12.57989064830760206 ) ) ;
#9320 = CARTESIAN_POINT ( 'NONE',  ( 1.861706995891666105, -10.38589138506421072, -6.878962591851865760 ) ) ;
#9321 = CARTESIAN_POINT ( 'NONE',  ( 0.3308579732647032867, -11.46737410776358779, 7.595989242675092790 ) ) ;
#9322 = B_SPLINE_CURVE_WITH_KNOTS ( 'NONE', 3,
 ( #6882, #15568, #17195, #5442 ),
 .UNSPECIFIED., .F., .F.,
 ( 4, 4 ),
 ( 1.779952243785056044E-16, 0.002004993803842976610 ),
 .UNSPECIFIED. ) ;
#9323 = ORIENTED_EDGE ( 'NONE', *, *, #4445, .T. ) ;
#9324 = VECTOR ( 'NONE', #18198, 1000.000000000000000 ) ;
#9325 = AXIS2_PLACEMENT_3D ( 'NONE', #18771, #8461, #6944 ) ;
#9326 = CARTESIAN_POINT ( 'NONE',  ( 1.847461586945730261, 7.286856109515200686, -10.08650590720928619 ) ) ;
#9327 = AXIS2_PLACEMENT_3D ( 'NONE', #3896, #11076, #18506 ) ;
#9328 = DIRECTION ( 'NONE',  ( 1.000000000000000000, 0.000000000000000000, 0.000000000000000000 ) ) ;
#9329 = CARTESIAN_POINT ( 'NONE',  ( 1.847372867223024295, -11.86627781945711568, 3.744745203533932365 ) ) ;
#9330 = LINE ( 'NONE', #18301, #6931 ) ;
#9331 = ORIENTED_EDGE ( 'NONE', *, *, #5354, .F. ) ;
#9332 = EDGE_CURVE ( 'NONE', #17964, #3017, #8430, .T. ) ;
#9333 = ORIENTED_EDGE ( 'NONE', *, *, #11989, .T. ) ;
#9334 = VERTEX_POINT ( 'NONE', #12916 ) ;
#9335 = ORIENTED_EDGE ( 'NONE', *, *, #5861, .T. ) ;
#9336 = VERTEX_POINT ( 'NONE', #12735 ) ;
#9337 = EDGE_CURVE ( 'NONE', #698, #15961, #10958, .T. ) ;
#9338 = AXIS2_PLACEMENT_3D ( 'NONE', #2149, #15142, #2557 ) ;
#9339 = VECTOR ( 'NONE', #17267, 1000.000000000000000 ) ;
#9340 = CARTESIAN_POINT ( 'NONE',  ( 1.847168016377981559, -12.44137401948661648, 0.1868244120189130053 ) ) ;
#9341 = CARTESIAN_POINT ( 'NONE',  ( -4.447775431366607357, -7.500000000000001776, -16.63307795419225954 ) ) ;
#9342 = CARTESIAN_POINT ( 'NONE',  ( 1.918918678667045352, 9.738328798462491775, -7.860057224348732774 ) ) ;
#9343 = CARTESIAN_POINT ( 'NONE',  ( 1.846138399168762101, -3.446241763652916124, -11.95493567637853971 ) ) ;
#9344 = PLANE ( 'NONE',  #17743 ) ;
#9345 = CARTESIAN_POINT ( 'NONE',  ( 16.56872352241294521, 0.009382111268606257298, -0.004564908236400254740 ) ) ;
#9346 = CARTESIAN_POINT ( 'NONE',  ( 2.636624412714236865, 1.966863607038798701E-15, 16.06066017081991149 ) ) ;
#9347 = DIRECTION ( 'NONE',  ( -0.000000000000000000, -0.000000000000000000, 1.000000000000000000 ) ) ;
#9348 = DIRECTION ( 'NONE',  ( 0.000000000000000000, 0.000000000000000000, 1.000000000000000000 ) ) ;
#9349 = ORIENTED_EDGE ( 'NONE', *, *, #8846, .F. ) ;
#9350 = VECTOR ( 'NONE', #4461, 1000.000000000000114 ) ;
#9351 = STYLED_ITEM ( 'NONE', ( #5968 ), #17679 ) ;
#9352 = ORIENTED_EDGE ( 'NONE', *, *, #10158, .F. ) ;
#9353 = VECTOR ( 'NONE', #7289, 1000.000000000000000 ) ;
#9354 = EDGE_CURVE ( 'NONE', #13704, #17922, #7294, .T. ) ;
#9355 = ORIENTED_EDGE ( 'NONE', *, *, #14218, .T. ) ;
#9356 = VERTEX_POINT ( 'NONE', #11590 ) ;
#9357 = PLANE ( 'NONE',  #13796 ) ;
#9358 = CARTESIAN_POINT ( 'NONE',  ( 0.4754618798421171855, 11.68486377711966639, 7.564402563418515690 ) ) ;
#9359 = CARTESIAN_POINT ( 'NONE',  ( 1.846138399168762101, -7.646096044339819819, -9.815003036200495856 ) ) ;
#9360 = DIRECTION ( 'NONE',  ( 0.7561779333270775005, -0.6322161072786965930, 0.1688126975276491026 ) ) ;
#9361 = CARTESIAN_POINT ( 'NONE',  ( 2.636624412715362631, -15.80357026013197519, 2.862162146984090327 ) ) ;
#9362 = ORIENTED_EDGE ( 'NONE', *, *, #15381, .F. ) ;
#9363 = CARTESIAN_POINT ( 'NONE',  ( 1.846613052777651198, 10.26230975746759810, 7.035606253495352291 ) ) ;
#9364 = FACE_OUTER_BOUND ( 'NONE', #10658, .T. ) ;
#9365 = CARTESIAN_POINT ( 'NONE',  ( -0.2286586286994273798, 7.499999999999998224, -13.03338879287367824 ) ) ;
#9366 = CARTESIAN_POINT ( 'NONE',  ( 1.845755665166726844, 11.67596932341234250, 4.296872077620717434 ) ) ;
#9367 = STYLED_ITEM ( 'NONE', ( #6740 ), #5341 ) ;
#9368 = CARTESIAN_POINT ( 'NONE',  ( 0.000000000000000000, 2.375000000000000444, 0.000000000000000000 ) ) ;
#9369 = DIRECTION ( 'NONE',  ( 0.000000000000000000, 0.000000000000000000, 1.000000000000000000 ) ) ;
#9370 = CARTESIAN_POINT ( 'NONE',  ( -194.9999999999999716, 4.999999999999973355, -2.000000000000000000 ) ) ;
#9371 = EDGE_LOOP ( 'NONE', ( #10290, #16530 ) ) ;
#9372 = AXIS2_PLACEMENT_3D ( 'NONE', #16158, #2850, #17491 ) ;
#9374 = ORIENTED_EDGE ( 'NONE', *, *, #5158, .F. ) ;
#9373 = FACE_OUTER_BOUND ( 'NONE', #12562, .T. ) ;
#9375 = CARTESIAN_POINT ( 'NONE',  ( 2.369999999999999662, 5.817072295949927426E-16, -4.750000000000000000 ) ) ;
#9376 = VECTOR ( 'NONE', #2240, 1000.000000000000114 ) ;
#9377 = ADVANCED_FACE ( 'NONE', ( #1457, #10054 ), #11228, .F. ) ;
#9378 = EDGE_CURVE ( 'NONE', #6482, #9203, #3632, .T. ) ;
#9379 = EDGE_CURVE ( 'NONE', #14747, #16257, #15698, .T. ) ;
#9380 = STYLED_ITEM ( 'NONE', ( #965 ), #6229 ) ;
#9381 = AXIS2_PLACEMENT_3D ( 'NONE', #9829, #8053, #13774 ) ;
#9382 = VERTEX_POINT ( 'NONE', #15687 ) ;
#9383 = CARTESIAN_POINT ( 'NONE',  ( 3.353306896162456585, 5.573563251762281290, -12.78841260990232165 ) ) ;
#9384 = PRODUCT_DEFINITION_SHAPE ( 'NONE', 'NONE',  #16076 ) ;
#9385 = CARTESIAN_POINT ( 'NONE',  ( -0.3372494957989286557, -7.500000000000000888, -14.22369192593361831 ) ) ;
#9386 = ORIENTED_EDGE ( 'NONE', *, *, #3071, .F. ) ;
#9387 = CARTESIAN_POINT ( 'NONE',  ( 16.56679352167444819, -0.008252760440870216679, 0.004277682826583264174 ) ) ;
#9388 = FACE_OUTER_BOUND ( 'NONE', #14870, .T. ) ;
#9389 = CARTESIAN_POINT ( 'NONE',  ( 1.845755665166724846, -11.67596932341231231, -4.296872077620800034 ) ) ;
#9390 = LINE ( 'NONE', #11106, #1366 ) ;
#9391 = AXIS2_PLACEMENT_3D ( 'NONE', #8155, #1056, #6898 ) ;
#9392 = CARTESIAN_POINT ( 'NONE',  ( 0.3137051932979792457, -7.698472063774386420, -11.37800749014139612 ) ) ;
#9393 = LINE ( 'NONE', #15223, #17757 ) ;
#9395 = VERTEX_POINT ( 'NONE', #2589 ) ;
#9394 = DIRECTION ( 'NONE',  ( 0.000000000000000000, 0.000000000000000000, -1.000000000000000000 ) ) ;
#9396 = CYLINDRICAL_SURFACE ( 'NONE', #15189, 5.000000000000004441 ) ;
#9397 = CIRCLE ( 'NONE', #15497, 4.999999999999997335 ) ;
#9398 = ORIENTED_EDGE ( 'NONE', *, *, #16532, .T. ) ;
#9399 = CARTESIAN_POINT ( 'NONE',  ( 0.3150686449036074754, -11.20479228691391604, -7.951193823202520328 ) ) ;
#9400 = CARTESIAN_POINT ( 'NONE',  ( 4.000000000000006217, 1.156482317317873500E-15, 7.000000000000000000 ) ) ;
#9401 = VERTEX_POINT ( 'NONE', #8432 ) ;
#9402 = ORIENTED_EDGE ( 'NONE', *, *, #17099, .T. ) ;
#9403 = CARTESIAN_POINT ( 'NONE',  ( 2.636624412715137922, 2.161493821597615828, 15.91454522070216093 ) ) ;
#9404 = EDGE_CURVE ( 'NONE', #10867, #204, #14270, .T. ) ;
#9405 = CARTESIAN_POINT ( 'NONE',  ( 2.697797270744668019, -7.053988368581781465, -11.26906156738834675 ) ) ;
#9406 = ADVANCED_FACE ( 'NONE', ( #5550 ), #15711, .T. ) ;
#9407 = ORIENTED_EDGE ( 'NONE', *, *, #5004, .T. ) ;
#9408 = CARTESIAN_POINT ( 'NONE',  ( 0.3058872367615230181, 13.24582953854925371, 3.664492643742809364 ) ) ;
#9409 = CARTESIAN_POINT ( 'NONE',  ( 2.636624412714236865, 15.91454522070173638, 2.161493821596668585 ) ) ;
#9410 = SURFACE_SIDE_STYLE ('',( #2409 ) ) ;
#9411 = LINE ( 'NONE', #9586, #10548 ) ;
#9412 = CARTESIAN_POINT ( 'NONE',  ( 3.512766787570729576, 7.127386085303022867, -13.25664064834469613 ) ) ;
#9413 = EDGE_CURVE ( 'NONE', #859, #2427, #18676, .T. ) ;
#9414 = CARTESIAN_POINT ( 'NONE',  ( 0.4754618798421167414, -0.7484603771385368587, 13.89949764182682301 ) ) ;
#9415 = SHAPE_DEFINITION_REPRESENTATION ( #42, #14858 ) ;
#9416 = CARTESIAN_POINT ( 'NONE',  ( 1.918921323896323639, 10.48468902844562578, -6.832782632379261756 ) ) ;
#9417 = CARTESIAN_POINT ( 'NONE',  ( 1.861706995891666105, 3.332865258614144732, -12.00328602385076593 ) ) ;
#9418 = ORIENTED_EDGE ( 'NONE', *, *, #11755, .F. ) ;
#9419 = AXIS2_PLACEMENT_3D ( 'NONE', #15502, #13880, #12357 ) ;
#9420 = CARTESIAN_POINT ( 'NONE',  ( 0.3137051932979775248, 3.805684345189972895, -13.20008686438101719 ) ) ;
#9421 = CARTESIAN_POINT ( 'NONE',  ( 3.950837973638676281, 13.10350451991840615, 6.316429227969512894 ) ) ;
#9422 = CARTESIAN_POINT ( 'NONE',  ( 1.918918678667074440, 12.49849921341423276, -0.6348738215465657975 ) ) ;
#9423 = CARTESIAN_POINT ( 'NONE',  ( 0.3307726912345200776, -7.596084275798974161, 11.46720933246395369 ) ) ;
#9424 = EDGE_CURVE ( 'NONE', #5701, #12401, #8900, .T. ) ;
#9425 = VERTEX_POINT ( 'NONE', #4611 ) ;
#9426 = ORIENTED_EDGE ( 'NONE', *, *, #13120, .T. ) ;
#9427 = EDGE_CURVE ( 'NONE', #2319, #13310, #13488, .T. ) ;
#9428 = ORIENTED_EDGE ( 'NONE', *, *, #1607, .F. ) ;
#9429 = EDGE_CURVE ( 'NONE', #14429, #2787, #18457, .T. ) ;
#9430 = VERTEX_POINT ( 'NONE', #3055 ) ;
#9431 = EDGE_LOOP ( 'NONE', ( #10205, #2530, #9075, #1493 ) ) ;
#9432 = B_SPLINE_CURVE_WITH_KNOTS ( 'NONE', 3,
 ( #18349, #15387, #3823, #9383, #7962, #866 ),
 .UNSPECIFIED., .F., .F.,
 ( 4, 2, 4 ),
 ( 0.000000000000000000, 0.001500839035891551355, 0.003001678071783102711 ),
 .UNSPECIFIED. ) ;
#9433 = B_SPLINE_CURVE_WITH_KNOTS ( 'NONE', 3,
 ( #4286, #17092, #5795, #3997, #9912, #15745 ),
 .UNSPECIFIED., .F., .F.,
 ( 4, 2, 4 ),
 ( 0.000000000000000000, 0.001500839035891551355, 0.003001678071783102711 ),
 .UNSPECIFIED. ) ;
#9434 = CARTESIAN_POINT ( 'NONE',  ( 0.3145729642390391323, 11.29233589755992639, 7.825496023201352180 ) ) ;
#9435 = CARTESIAN_POINT ( 'NONE',  ( 16.57605080000000086, 6.799999999999999822, -1.500000000000000000 ) ) ;
#9436 = CARTESIAN_POINT ( 'NONE',  ( 1.845755665166724846, -3.386720041070645948, -11.97169564665394681 ) ) ;
#9437 = CARTESIAN_POINT ( 'NONE',  ( 2.320521194582656488, -7.743190876766163022, 13.71278319228045284 ) ) ;
#9438 = ADVANCED_FACE ( 'NONE', ( #11679 ), #8397, .F. ) ;
#9439 = CARTESIAN_POINT ( 'NONE',  ( 0.4862570985993252548, -5.003653737315580052, 12.97920246947877665 ) ) ;
#9440 = CARTESIAN_POINT ( 'NONE',  ( 1.254009781011253821, 14.24044713813288254, 3.563484327698356324 ) ) ;
#9441 = CARTESIAN_POINT ( 'NONE',  ( 14.99999999999999289, 15.00000000000000000, 3.000000000000000000 ) ) ;
#9442 = B_SPLINE_CURVE_WITH_KNOTS ( 'NONE', 3,
 ( #2192, #7946, #9725, #3528, #2107, #667 ),
 .UNSPECIFIED., .F., .F.,
 ( 4, 2, 4 ),
 ( 5.421010862427522170E-20, 0.0001828790815886950779, 0.0003657581631773901016 ),
 .UNSPECIFIED. ) ;
#9443 = CARTESIAN_POINT ( 'NONE',  ( 0.3137051932979792457, 8.442169467527008919, -10.83767969834794087 ) ) ;
#9444 = CARTESIAN_POINT ( 'NONE',  ( 0.3058872367615230181, -11.46514199369352482, -7.578326039752732335 ) ) ;
#9445 = ORIENTED_EDGE ( 'NONE', *, *, #9317, .T. ) ;
#9446 = EDGE_LOOP ( 'NONE', ( #15338, #6785, #9097, #2243 ) ) ;
#9447 = EDGE_LOOP ( 'NONE', ( #9846, #8872, #9754, #7052 ) ) ;
#9448 = ORIENTED_EDGE ( 'NONE', *, *, #8910, .F. ) ;
#9449 = B_SPLINE_CURVE_WITH_KNOTS ( 'NONE', 3,
 ( #10323, #16151, #3033, #8881, #1620, #7464 ),
 .UNSPECIFIED., .F., .F.,
 ( 4, 2, 4 ),
 ( 7.047314121155778821E-19, 0.001657017934712349183, 0.003314035869424697932 ),
 .UNSPECIFIED. ) ;
#9450 = DIRECTION ( 'NONE',  ( 0.000000000000000000, 1.000000000000000000, 1.224646799147353454E-16 ) ) ;
#9451 = CARTESIAN_POINT ( 'NONE',  ( 1.342453679581834924, 12.51077660954477189, -7.902645620902311485 ) ) ;
#9452 = LINE ( 'NONE', #13836, #12361 ) ;
#9453 = CARTESIAN_POINT ( 'NONE',  ( 16.57210152137263393, 0.008007331252332874558, 0.01214401161737521141 ) ) ;
#9454 = AXIS2_PLACEMENT_3D ( 'NONE', #4465, #10194, #4659 ) ;
#9455 = CARTESIAN_POINT ( 'NONE',  ( 0.3132635586635996727, 13.21855946425836592, 3.740017578711807289 ) ) ;
#9456 = EDGE_LOOP ( 'NONE', ( #13976, #8712, #11857, #9119 ) ) ;
#9457 = VECTOR ( 'NONE', #13394, 1000.000000000000000 ) ;
#9458 = CARTESIAN_POINT ( 'NONE',  ( 0.8740779401507015045, 14.27348745891557158, -0.8420120399581809689 ) ) ;
#9459 = ADVANCED_FACE ( 'NONE', ( #14639 ), #14727, .T. ) ;
#9460 = CARTESIAN_POINT ( 'NONE',  ( 16.57778382496167424, -0.006312874906843954532, -0.01354073047775891311 ) ) ;
#9461 = CARTESIAN_POINT ( 'NONE',  ( -5.075684663107223216, 4.834325206103791572, -12.00000000445675319 ) ) ;
#9462 = CARTESIAN_POINT ( 'NONE',  ( 2.636624412716062071, -11.10302021258080352, -11.60464335004061454 ) ) ;
#9463 = MECHANICAL_DESIGN_GEOMETRIC_PRESENTATION_REPRESENTATION (  '', ( #17705 ), #1202 ) ;
#9464 = DIRECTION ( 'NONE',  ( -1.000000000000000000, 0.000000000000000000, 0.000000000000000000 ) ) ;
#9465 = ADVANCED_FACE ( 'NONE', ( #6046 ), #313, .F. ) ;
#9466 = CARTESIAN_POINT ( 'NONE',  ( 0.8740764193771586310, 12.04241474978035420, -7.708542792189425619 ) ) ;
#9467 = EDGE_LOOP ( 'NONE', ( #7342, #8824, #4862, #13285 ) ) ;
#9469 = ORIENTED_EDGE ( 'NONE', *, *, #700, .F. ) ;
#9468 = CARTESIAN_POINT ( 'NONE',  ( 1.846524061778019421, 11.93805390544205913, -3.506196582970981357 ) ) ;
#9470 = CARTESIAN_POINT ( 'NONE',  ( 1.861706995891668326, 11.66987142852990189, -4.359009869687124450 ) ) ;
#9471 = ORIENTED_EDGE ( 'NONE', *, *, #1262, .F. ) ;
#9472 = CARTESIAN_POINT ( 'NONE',  ( 1.847168016377986000, -4.022276579849877187, -11.77471791462002670 ) ) ;
#9473 = B_SPLINE_CURVE_WITH_KNOTS ( 'NONE', 3,
 ( #18507, #5858, #14751, #9027 ),
 .UNSPECIFIED., .F., .F.,
 ( 4, 4 ),
 ( 0.000000000000000000, 0.002004993803842618390 ),
 .UNSPECIFIED. ) ;
#9474 = CARTESIAN_POINT ( 'NONE',  ( -5.250594443111816112, -4.638468187398823162, -11.99999999738842682 ) ) ;
#9475 = VERTEX_POINT ( 'NONE', #406 ) ;
#9476 = CARTESIAN_POINT ( 'NONE',  ( 1.847372867223025406, -7.398914411685061587, 10.00438561114521185 ) ) ;
#9477 = CARTESIAN_POINT ( 'NONE',  ( 3.377929128793398572, 3.070552481925057364, -13.64476897106781017 ) ) ;
#9478 = CARTESIAN_POINT ( 'NONE',  ( 1.846138399168762101, -11.69739621335919111, -4.238866729160527314 ) ) ;
#9479 = CARTESIAN_POINT ( 'NONE',  ( 0.000000000000000000, 0.000000000000000000, 10.00000000000000000 ) ) ;
#9480 = ADVANCED_FACE ( 'NONE', ( #16073 ), #13195, .F. ) ;
#9481 = EDGE_CURVE ( 'NONE', #8310, #6145, #10714, .T. ) ;
#9482 = EDGE_CURVE ( 'NONE', #31, #3117, #1352, .T. ) ;
#9483 = DIRECTION ( 'NONE',  ( -0.7635533937278216055, -0.2197766120036420967, -0.6071939193889598352 ) ) ;
#9484 = CARTESIAN_POINT ( 'NONE',  ( 0.3720661004400040439, -10.73619472937708252, 8.694226082900557984 ) ) ;
#9486 = ORIENTED_EDGE ( 'NONE', *, *, #13170, .F. ) ;
#9485 = PLANE ( 'NONE',  #6844 ) ;
#9487 = LINE ( 'NONE', #2220, #6027 ) ;
#9488 = CARTESIAN_POINT ( 'NONE',  ( 0.3095370825347224519, 3.806662003783598536, -13.20347358821910433 ) ) ;
#9489 = CARTESIAN_POINT ( 'NONE',  ( 1.959212340397942231, 12.12975361829680310, -3.239239832448903122 ) ) ;
#9490 = CARTESIAN_POINT ( 'NONE',  ( 1.254255976357310010, 7.789651112956863521, 12.44256109021772438 ) ) ;
#9491 = ORIENTED_EDGE ( 'NONE', *, *, #11670, .F. ) ;
#9492 = ORIENTED_EDGE ( 'NONE', *, *, #4123, .T. ) ;
#9493 = CARTESIAN_POINT ( 'NONE',  ( -112.9592833967653149, -82.42962774651277869, -85.91158569379400944 ) ) ;
#9494 = CARTESIAN_POINT ( 'NONE',  ( -59.99999999999997158, -25.00000000000000711, 3.000000000000000000 ) ) ;
#9495 = ADVANCED_FACE ( 'NONE', ( #5838 ), #2002, .T. ) ;
#9496 = ORIENTED_EDGE ( 'NONE', *, *, #4539, .F. ) ;
#9497 = AXIS2_PLACEMENT_3D ( 'NONE', #6972, #17269, #7153 ) ;
#9498 = DIRECTION ( 'NONE',  ( 0.000000000000000000, 0.000000000000000000, -1.000000000000000000 ) ) ;
#9499 = LINE ( 'NONE', #6364, #12129 ) ;
#9500 = CARTESIAN_POINT ( 'NONE',  ( 2.320521194582656932, -14.32454473829943886, 6.542541239685230714 ) ) ;
#9501 = PRODUCT_CONTEXT ( 'NONE', #12898, 'mechanical' ) ;
#9502 = EDGE_CURVE ( 'NONE', #16237, #14846, #17866, .T. ) ;
#9503 = DIRECTION ( 'NONE',  ( 0.4246593920385850485, 0.1376957914266804250, -0.8948208031649687033 ) ) ;
#9504 = CARTESIAN_POINT ( 'NONE',  ( 1.254255976357895763, -3.563435620217493494, -14.24071337840814166 ) ) ;
#9505 = ADVANCED_FACE ( 'NONE', ( #8147 ), #16745, .T. ) ;
#9506 = CARTESIAN_POINT ( 'NONE',  ( 0.3137051932979792457, 7.698472063774471685, 11.37800749014133928 ) ) ;
#9507 = DIRECTION ( 'NONE',  ( 0.000000000000000000, 0.000000000000000000, 1.000000000000000000 ) ) ;
#9508 = AXIS2_PLACEMENT_3D ( 'NONE', #1849, #7689, #15306 ) ;
#9509 = CARTESIAN_POINT ( 'NONE',  ( 3.950837973638676281, -12.81214529934979929, 6.888253895133251703 ) ) ;
#9510 = FACE_OUTER_BOUND ( 'NONE', #11819, .T. ) ;
#9511 = ORIENTED_EDGE ( 'NONE', *, *, #8168, .T. ) ;
#9512 = EDGE_CURVE ( 'NONE', #12401, #18780, #9390, .T. ) ;
#9513 = ORIENTED_EDGE ( 'NONE', *, *, #7089, .T. ) ;
#9514 = ORIENTED_EDGE ( 'NONE', *, *, #9379, .F. ) ;
#9515 = ORIENTED_EDGE ( 'NONE', *, *, #10653, .F. ) ;
#9516 = VERTEX_POINT ( 'NONE', #9658 ) ;
#9517 = CARTESIAN_POINT ( 'NONE',  ( 0.3132635586635976188, 0.5277914263193109745, 13.72732610560088773 ) ) ;
#9518 = CARTESIAN_POINT ( 'NONE',  ( -0.5553368343811752039, -7.500000000000002665, -14.29382045140262036 ) ) ;
#9519 = EDGE_LOOP ( 'NONE', ( #16483, #2717, #15445, #705 ) ) ;
#9520 = CARTESIAN_POINT ( 'NONE',  ( 1.845755665166723736, -12.43231320373360482, -0.4784952423729852966 ) ) ;
#9521 = CARTESIAN_POINT ( 'NONE',  ( 1.342453679581834924, 14.76648944001039254, 0.9602753779831241232 ) ) ;
#9522 = CARTESIAN_POINT ( 'NONE',  ( 2.636624412715137922, -6.973567714907947135, 14.46769361191283920 ) ) ;
#9523 = CARTESIAN_POINT ( 'NONE',  ( 3.664313757352973600, -12.42002390572631221, 7.012524439851453906 ) ) ;
#9524 = CARTESIAN_POINT ( 'NONE',  ( 2.705023505549862151, -12.88681800078730255, -3.294610156756031305 ) ) ;
#9525 = ADVANCED_FACE ( 'NONE', ( #10728, #13961 ), #13778, .F. ) ;
#9526 = VECTOR ( 'NONE', #16753, 1000.000000000000000 ) ;
#9527 = CARTESIAN_POINT ( 'NONE',  ( -194.9999999999999716, 14.99999999999997513, 6.000000000000005329 ) ) ;
#9528 = CARTESIAN_POINT ( 'NONE',  ( 16.56782317627811096, 0.003357783021327817585, 0.009228812961908668469 ) ) ;
#9529 = VERTEX_POINT ( 'NONE', #18355 ) ;
#9530 = EDGE_LOOP ( 'NONE', ( #18785, #14070, #7399, #11055 ) ) ;
#9531 = ORIENTED_EDGE ( 'NONE', *, *, #6837, .T. ) ;
#9532 = ORIENTED_EDGE ( 'NONE', *, *, #13952, .F. ) ;
#9533 = CARTESIAN_POINT ( 'NONE',  ( 16.56872352241294521, 0.007240717549633990044, -0.007512283835805476720 ) ) ;
#9534 = CARTESIAN_POINT ( 'NONE',  ( 3.664313757352971379, -1.627055439596372777, 14.16986885736092461 ) ) ;
#9535 = CARTESIAN_POINT ( 'NONE',  ( 1.846822687350015757, -7.075150813727044685, -10.23524390843947529 ) ) ;
#9536 = CARTESIAN_POINT ( 'NONE',  ( 16.58200780006414732, -0.002844973367391502410, 0.01080144354108869553 ) ) ;
#9537 = CIRCLE ( 'NONE', #4962, 0.2000000000000000944 ) ;
#9538 = CARTESIAN_POINT ( 'NONE',  ( 16.56782317627811096, 0.0003415813796006246777, -0.009814734722107084502 ) ) ;
#9539 = ORIENTED_EDGE ( 'NONE', *, *, #12186, .T. ) ;
#9540 = CARTESIAN_POINT ( 'NONE',  ( 1.560000000000000053, -1.299038105676658450, 0.7500000000000007772 ) ) ;
#9541 = CARTESIAN_POINT ( 'NONE',  ( 16.58200780006414732, -0.008650561019685852962, -0.007066318000005976374 ) ) ;
#9542 = CARTESIAN_POINT ( 'NONE',  ( 0.9371186270715102795, 6.939831204821730104, -11.99999999628260561 ) ) ;
#9543 = CARTESIAN_POINT ( 'NONE',  ( 2.636624412716061627, -7.605649742761058540, -14.14563173255469408 ) ) ;
#9544 = AXIS2_PLACEMENT_3D ( 'NONE', #5131, #10973, #16794 ) ;
#9545 = CARTESIAN_POINT ( 'NONE',  ( 3.950837973638675393, -13.10350451991835818, -6.316429227969608817 ) ) ;
#9546 = CARTESIAN_POINT ( 'NONE',  ( 1.562796894703937678, 0.000000000000000000, 0.000000000000000000 ) ) ;
#9547 = DIRECTION ( 'NONE',  ( 0.000000000000000000, 0.000000000000000000, -1.000000000000000000 ) ) ;
#9548 = CARTESIAN_POINT ( 'NONE',  ( 3.664313757352979373, 13.97913389346637736, -2.831308606787096949 ) ) ;
#9549 = ORIENTED_EDGE ( 'NONE', *, *, #13607, .T. ) ;
#9551 = ORIENTED_EDGE ( 'NONE', *, *, #11670, .T. ) ;
#9550 = CARTESIAN_POINT ( 'NONE',  ( 0.3170788640506440603, 11.02668139258442359, 8.200855617524574370 ) ) ;
#9552 = CARTESIAN_POINT ( 'NONE',  ( 16.57210152137263393, 0.0006600038696346007027, -0.01453130299868522768 ) ) ;
#9553 = EDGE_CURVE ( 'NONE', #17458, #17275, #454, .T. ) ;
#9554 = CYLINDRICAL_SURFACE ( 'NONE', #16852, 2.499999999999995115 ) ;
#9555 = CIRCLE ( 'NONE', #16276, 1.500000000000000000 ) ;
#9556 = VERTEX_POINT ( 'NONE', #7969 ) ;
#9557 = CARTESIAN_POINT ( 'NONE',  ( 0.000000000000000000, 0.000000000000000000, 0.000000000000000000 ) ) ;
#9558 = CARTESIAN_POINT ( 'NONE',  ( -3.253466017772906227, -7.500000000000001776, -13.21345932477064444 ) ) ;
#9559 = ORIENTED_EDGE ( 'NONE', *, *, #13442, .F. ) ;
#9560 = CARTESIAN_POINT ( 'NONE',  ( 3.074695600507237891, -15.41438262616227739, 2.093687500611889352 ) ) ;
#9561 = CARTESIAN_POINT ( 'NONE',  ( 2.636624412715362631, -15.80357026013197519, 2.862162146984090327 ) ) ;
#9562 = CARTESIAN_POINT ( 'NONE',  ( 0.3307726912345178572, 7.596084275799059427, -11.46720933246390572 ) ) ;
#9563 = CARTESIAN_POINT ( 'NONE',  ( 1.847412631396500249, 10.09191835241973934, -7.278870946904142158 ) ) ;
#9564 = VECTOR ( 'NONE', #2667, 1000.000000000000114 ) ;
#9565 = FILL_AREA_STYLE ('',( #8243 ) ) ;
#9566 = VECTOR ( 'NONE', #10091, 1000.000000000000114 ) ;
#9567 = CARTESIAN_POINT ( 'NONE',  ( 2.747332970342022840, -14.63517873738952524, 7.289199830147050641 ) ) ;
#9568 =( BOUNDED_SURFACE ( )  B_SPLINE_SURFACE ( 3, 1, ( 
 ( #4595, #3135 ),
 ( #10418, #3607 ),
 ( #835, #5036 ),
 ( #1822, #16254 ) ),
 .UNSPECIFIED., .F., .F., .T. ) 
 B_SPLINE_SURFACE_WITH_KNOTS ( ( 4, 4 ),
 ( 2, 2 ),
 ( 0.000000000000000000, 1.000000000000000000 ),
 ( 0.000000000000000000, 1.000000000000000000 ),
 .UNSPECIFIED. ) 
 GEOMETRIC_REPRESENTATION_ITEM ( )  RATIONAL_B_SPLINE_SURFACE ( (
 ( 1.000000000000000000, 1.000000000000000000),
 ( 0.9593108457356467333, 0.9995965569486454649),
 ( 0.9593108457356467333, 0.9995965569486454649),
 ( 1.000000000000000000, 1.000000000000000000) ) ) 
 REPRESENTATION_ITEM ( '' )  SURFACE ( )  );
#9569 = FACE_BOUND ( 'NONE', #1226, .T. ) ;
#9570 = ORIENTED_EDGE ( 'NONE', *, *, #10809, .F. ) ;
#9571 = CARTESIAN_POINT ( 'NONE',  ( 2.002547531651520885, -4.532360870844412304, 11.75462648437100377 ) ) ;
#9572 = ORIENTED_EDGE ( 'NONE', *, *, #10653, .T. ) ;
#9573 = FACE_OUTER_BOUND ( 'NONE', #11742, .T. ) ;
#9574 = CARTESIAN_POINT ( 'NONE',  ( 16.56753206892534891, 0.006669401563384923064, -0.006760771273036194837 ) ) ;
#9575 = ORIENTED_EDGE ( 'NONE', *, *, #8646, .F. ) ;
#9576 = EDGE_CURVE ( 'NONE', #15271, #10362, #6430, .T. ) ;
#9577 = ORIENTED_EDGE ( 'NONE', *, *, #11899, .F. ) ;
#9578 = CARTESIAN_POINT ( 'NONE',  ( 0.000000000000000000, 0.000000000000000000, 11.00000000000000000 ) ) ;
#9579 = CARTESIAN_POINT ( 'NONE',  ( 0.3058872367615230181, 11.46514199369357989, 7.578326039752647958 ) ) ;
#9580 = VERTEX_POINT ( 'NONE', #6523 ) ;
#9581 = CARTESIAN_POINT ( 'NONE',  ( 16.57210152137263393, -0.01402404281922924566, 0.003862718596009228310 ) ) ;
#9582 = CARTESIAN_POINT ( 'NONE',  ( -55.93192566395838128, 4.999999999999974243, 6.000000000000000000 ) ) ;
#9583 = MECHANICAL_DESIGN_GEOMETRIC_PRESENTATION_REPRESENTATION (  '', ( #17798 ), #15669 ) ;
#9584 = DIRECTION ( 'NONE',  ( -1.913297951445007622E-16, 1.000000000000000000, 0.000000000000000000 ) ) ;
#9585 = PRODUCT_DEFINITION_FORMATION_WITH_SPECIFIED_SOURCE ( 'ANY', '', #7466, .NOT_KNOWN. ) ;
#9586 = CARTESIAN_POINT ( 'NONE',  ( 15.00000000000000711, -14.99999999999999645, 8.000000000000000000 ) ) ;
#9587 = CARTESIAN_POINT ( 'NONE',  ( 3.512766787570761107, 14.91422000116819468, -2.025881399556438200 ) ) ;
#9588 = CARTESIAN_POINT ( 'NONE',  ( 3.950837973638676281, 1.958075594453990487, -14.41405733518058341 ) ) ;
#9589 = APPLICATION_PROTOCOL_DEFINITION ( 'draft international standard', 'automotive_design', 1998, #11932 ) ;
#9590 = LINE ( 'NONE', #6650, #16884 ) ;
#9591 = DIRECTION ( 'NONE',  ( -0.000000000000000000, -0.000000000000000000, 1.000000000000000000 ) ) ;
#9592 = CARTESIAN_POINT ( 'NONE',  ( 8.522092701127531811, -0.3779863304871711183, 6.946128462138593918 ) ) ;
#9593 = DIRECTION ( 'NONE',  ( 0.000000000000000000, 1.000000000000000000, 0.000000000000000000 ) ) ;
#9594 = PLANE ( 'NONE',  #2647 ) ;
#9595 = CARTESIAN_POINT ( 'NONE',  ( 0.3170788640506440603, -4.392045232375903829, 13.02120094575826670 ) ) ;
#9596 = ORIENTED_EDGE ( 'NONE', *, *, #7556, .F. ) ;
#9597 = AXIS2_PLACEMENT_3D ( 'NONE', #17102, #4104, #7071 ) ;
#9598 = EDGE_CURVE ( 'NONE', #15937, #11936, #2036, .T. ) ;
#9599 = EDGE_CURVE ( 'NONE', #13920, #18879, #15423, .T. ) ;
#9600 = ORIENTED_EDGE ( 'NONE', *, *, #9217, .T. ) ;
#9601 = AXIS2_PLACEMENT_3D ( 'NONE', #5682, #15629, #7241 ) ;
#9602 = ORIENTED_EDGE ( 'NONE', *, *, #16891, .T. ) ;
#9603 = ORIENTED_EDGE ( 'NONE', *, *, #5563, .T. ) ;
#9604 = SHAPE_REPRESENTATION ( 'cutting support', ( #2030 ), #5382 ) ;
#9605 = CARTESIAN_POINT ( 'NONE',  ( 1.846955891736116184, -0.2634721419534329923, -12.44001089941741611 ) ) ;
#9606 = CARTESIAN_POINT ( 'NONE',  ( 6.538348415311014072, -7.500000000000000888, -16.99999999999999645 ) ) ;
#9607 = APPLICATION_CONTEXT ( 'automotive_design' ) ;
#9608 = AXIS2_PLACEMENT_3D ( 'NONE', #7388, #4519, #1743 ) ;
#9609 = CARTESIAN_POINT ( 'NONE',  ( 16.56753206892534891, 0.001549402974394163733, 0.009369540855502535986 ) ) ;
#9610 = DIRECTION ( 'NONE',  ( -0.000000000000000000, 0.000000000000000000, 1.000000000000000000 ) ) ;
#9611 = CIRCLE ( 'NONE', #4426, 1.500000000000000000 ) ;
#9612 = CIRCLE ( 'NONE', #12069, 16.06066017081991149 ) ;
#9613 = FACE_OUTER_BOUND ( 'NONE', #9447, .T. ) ;
#9614 = CARTESIAN_POINT ( 'NONE',  ( 0.3137051932979757485, 13.73004976592202020, -0.4596302728640235258 ) ) ;
#9615 = CARTESIAN_POINT ( 'NONE',  ( 0.4862570985993235340, -7.559321496869339185, -11.67702470553373750 ) ) ;
#9616 = CARTESIAN_POINT ( 'NONE',  ( 16.56753206892534891, -0.009389754735541561842, 0.001421777558676752366 ) ) ;
#9617 = CARTESIAN_POINT ( 'NONE',  ( 2.353870697619109720, 10.90705766126230536, -6.980654702310723714 ) ) ;
#9618 = ORIENTED_EDGE ( 'NONE', *, *, #12485, .T. ) ;
#9619 = EDGE_LOOP ( 'NONE', ( #183, #12396, #16288, #8911 ) ) ;
#9620 = ORIENTED_EDGE ( 'NONE', *, *, #11622, .F. ) ;
#9621 = CIRCLE ( 'NONE', #13906, 14.54644660717763927 ) ;
#9622 = VERTEX_POINT ( 'NONE', #16563 ) ;
#9623 = AXIS2_PLACEMENT_3D ( 'NONE', #1990, #18130, #16524 ) ;
#9624 = B_SPLINE_CURVE_WITH_KNOTS ( 'NONE', 3,
 ( #5719, #11040, #15326, #897, #9500, #13089 ),
 .UNSPECIFIED., .F., .F.,
 ( 4, 2, 4 ),
 ( 1.305552300251627978E-18, 0.001657017934710633541, 0.003314035869421265781 ),
 .UNSPECIFIED. ) ;
#9625 = CARTESIAN_POINT ( 'NONE',  ( 8.438534575730034959, 6.862570336891075762, -0.2320579683290367456 ) ) ;
#9626 = EDGE_CURVE ( 'NONE', #13108, #1712, #1107, .T. ) ;
#9627 = CARTESIAN_POINT ( 'NONE',  ( 0.3058872367615226295, -13.24582953854928036, 3.664492643742712108 ) ) ;
#9628 = CARTESIAN_POINT ( 'NONE',  ( 0.3095370825347224519, -13.73357284481724427, -0.4597470195091612477 ) ) ;
#9629 = DIRECTION ( 'NONE',  ( 0.000000000000000000, 0.000000000000000000, -1.000000000000000000 ) ) ;
#9630 = CARTESIAN_POINT ( 'NONE',  ( 16.57210152137263393, 0.01453130299868640209, -0.0006600038696348341314 ) ) ;
#9631 = ORIENTED_EDGE ( 'NONE', *, *, #7390, .T. ) ;
#9632 = CARTESIAN_POINT ( 'NONE',  ( 16.56782317627811096, 0.0003415813796014688375, 0.009814734722106369796 ) ) ;
#9633 = DIRECTION ( 'NONE',  ( -0.7561779333270775005, -0.5491072561318312006, -0.3559159372837374935 ) ) ;
#9634 = CARTESIAN_POINT ( 'NONE',  ( -0.3417098569969649335, 7.499999999999999112, -14.22469181348822431 ) ) ;
#9635 = CARTESIAN_POINT ( 'NONE',  ( 0.4385251269669948049, 13.84299131624729817, 0.7363879510385874516 ) ) ;
#9636 = CARTESIAN_POINT ( 'NONE',  ( 2.636624412714236865, 0.000000000000000000, 0.000000000000000000 ) ) ;
#9637 = CARTESIAN_POINT ( 'NONE',  ( 1.977436885027412439, 13.27782258182005748, -7.806953934146017460 ) ) ;
#9638 = VECTOR ( 'NONE', #7322, 1000.000000000000000 ) ;
#9639 = MECHANICAL_DESIGN_GEOMETRIC_PRESENTATION_REPRESENTATION (  '', ( #9351 ), #7207 ) ;
#9640 = CARTESIAN_POINT ( 'NONE',  ( 0.3137051932979809665, 10.83767969834803324, 8.442169467526891680 ) ) ;
#9641 = ORIENTED_EDGE ( 'NONE', *, *, #3804, .F. ) ;
#9643 = ORIENTED_EDGE ( 'NONE', *, *, #4070, .F. ) ;
#9642 = DIRECTION ( 'NONE',  ( 0.000000000000000000, 1.000000000000000000, -0.000000000000000000 ) ) ;
#9644 = CARTESIAN_POINT ( 'NONE',  ( 0.3137051932979792457, -10.83767969834809008, 8.442169467526815296 ) ) ;
#9645 = PRODUCT_DEFINITION ( 'UNKNOWN', '', #12938, #1986 ) ;
#9646 = ADVANCED_FACE ( 'NONE', ( #8056 ), #12256, .T. ) ;
#9647 = DIRECTION ( 'NONE',  ( 0.000000000000000000, 0.000000000000000000, 1.000000000000000000 ) ) ;
#9648 = EDGE_LOOP ( 'NONE', ( #10575, #7316, #17058, #3047 ) ) ;
#9649 = CARTESIAN_POINT ( 'NONE',  ( 0.3137051932979792457, -11.37800749014136592, 7.698472063774431717 ) ) ;
#9650 = EDGE_CURVE ( 'NONE', #1657, #8563, #14809, .T. ) ;
#9651 = CIRCLE ( 'NONE', #12108, 14.54644660717763927 ) ;
#9652 = EDGE_LOOP ( 'NONE', ( #9532, #1112, #14088, #12226 ) ) ;
#9653 = CARTESIAN_POINT ( 'NONE',  ( 1.846613052777651198, -12.43780859207240042, 0.3401093050881381363 ) ) ;
#9654 = ORIENTED_EDGE ( 'NONE', *, *, #12824, .T. ) ;
#9655 = DIRECTION ( 'NONE',  ( 1.224646799147353207E-16, 1.000000000000000000, -0.000000000000000000 ) ) ;
#9656 = CARTESIAN_POINT ( 'NONE',  ( 0.3137051932979757485, 13.73004976592202020, -0.4596302728640235258 ) ) ;
#9657 = DIRECTION ( 'NONE',  ( 0.000000000000000000, 0.000000000000000000, 1.000000000000000000 ) ) ;
#9658 = CARTESIAN_POINT ( 'NONE',  ( 0.3137051932979792457, -8.442169467526928983, 10.83767969834800127 ) ) ;
#9659 = CARTESIAN_POINT ( 'NONE',  ( 1.428504764830155575E-14, -7.013167318348350499, 33.78111653772643308 ) ) ;
#9660 = VECTOR ( 'NONE', #11003, 1000.000000000000114 ) ;
#9661 = B_SPLINE_CURVE_WITH_KNOTS ( 'NONE', 3,
 ( #1406, #16128, #7538, #18889 ),
 .UNSPECIFIED., .F., .F.,
 ( 4, 4 ),
 ( 0.000000000000000000, 0.002004993803841946618 ),
 .UNSPECIFIED. ) ;
#9662 = ADVANCED_FACE ( 'NONE', ( #13864 ), #11014, .F. ) ;
#9663 = CIRCLE ( 'NONE', #11207, 5.000000000000000000 ) ;
#9664 = CARTESIAN_POINT ( 'NONE',  ( 2.002547531651519996, 12.57989064830759496, -0.6781519942172177240 ) ) ;
#9665 = PRESENTATION_LAYER_ASSIGNMENT (  '', '', ( #6327 ) ) ;
#9666 = DIRECTION ( 'NONE',  ( 0.000000000000000000, 0.000000000000000000, 1.000000000000000000 ) ) ;
#9668 = EDGE_LOOP ( 'NONE', ( #80, #9559, #15831, #10037 ) ) ;
#9667 = CARTESIAN_POINT ( 'NONE',  ( 0.000000000000000000, 0.000000000000000000, -6.000000000000000000 ) ) ;
#9669 = CARTESIAN_POINT ( 'NONE',  ( 0.3095370825347224519, -11.38092634279622928, -7.700448427571997989 ) ) ;
#9670 = CIRCLE ( 'NONE', #6628, 5.000000000000000888 ) ;
#9671 = CARTESIAN_POINT ( 'NONE',  ( 0.3145729642390400205, -11.29233589755986600, -7.825496023201434781 ) ) ;
#9672 = DIRECTION ( 'NONE',  ( 0.000000000000000000, -1.040834085586084257E-15, -1.000000000000000000 ) ) ;
#9673 = EDGE_LOOP ( 'NONE', ( #5496, #1337, #2901, #11219 ) ) ;
#9674 = ORIENTED_EDGE ( 'NONE', *, *, #11432, .F. ) ;
#9675 = LINE ( 'NONE', #12625, #7838 ) ;
#9676 = VECTOR ( 'NONE', #12245, 1000.000000000000000 ) ;
#9677 = DIRECTION ( 'NONE',  ( 1.000000000000000000, 0.000000000000000000, 0.000000000000000000 ) ) ;
#9678 = VERTEX_POINT ( 'NONE', #5170 ) ;
#9679 = CARTESIAN_POINT ( 'NONE',  ( 1.861706995891673433, -0.5394761475744983548, -12.44571539481144562 ) ) ;
#9680 = CIRCLE ( 'NONE', #3881, 2.100000000000000977 ) ;
#9681 = CARTESIAN_POINT ( 'NONE',  ( 1.918918678667043354, 10.48466773720562273, 6.832809802519053122 ) ) ;
#9682 = CARTESIAN_POINT ( 'NONE',  ( 2.123976203522053741, -13.47898556379307244, -7.899625852120357727 ) ) ;
#9683 = CARTESIAN_POINT ( 'NONE',  ( 1.560000000000000053, 0.000000000000000000, 2.999999999999998668 ) ) ;
#9684 = DIRECTION ( 'NONE',  ( -1.000000000000000000, 0.000000000000000000, 0.000000000000000000 ) ) ;
#9685 = EDGE_CURVE ( 'NONE', #9139, #7697, #8205, .T. ) ;
#9686 = FILL_AREA_STYLE ('',( #15865 ) ) ;
#9687 = SHAPE_DEFINITION_REPRESENTATION ( #16065, #9113 ) ;
#9688 =( BOUNDED_SURFACE ( )  B_SPLINE_SURFACE ( 3, 1, ( 
 ( #6239, #4989 ),
 ( #4811, #1846 ),
 ( #9106, #17809 ),
 ( #6528, #4712 ) ),
 .UNSPECIFIED., .F., .F., .T. ) 
 B_SPLINE_SURFACE_WITH_KNOTS ( ( 4, 4 ),
 ( 2, 2 ),
 ( 0.000000000000000000, 1.000000000000000000 ),
 ( 0.000000000000000000, 1.000000000000000000 ),
 .UNSPECIFIED. ) 
 GEOMETRIC_REPRESENTATION_ITEM ( )  RATIONAL_B_SPLINE_SURFACE ( (
 ( 1.000000000000000000, 1.000000000000000000),
 ( 0.7792777138730160313, 0.9689936506012927220),
 ( 0.7792777138730160313, 0.9689936506012927220),
 ( 1.000000000000000000, 1.000000000000000000) ) ) 
 REPRESENTATION_ITEM ( '' )  SURFACE ( )  );
#9689 =( NAMED_UNIT ( * ) SI_UNIT ( $, .STERADIAN. ) SOLID_ANGLE_UNIT ( ) );
#9690 = CARTESIAN_POINT ( 'NONE',  ( 0.4862570985993252548, 13.44146924561381162, 3.580942890621718888 ) ) ;
#9691 = EDGE_CURVE ( 'NONE', #17807, #18257, #13201, .T. ) ;
#9692 = CARTESIAN_POINT ( 'NONE',  ( 0.3058872367615226295, -12.87003593440624982, -4.821066432589462103 ) ) ;
#9693 = CARTESIAN_POINT ( 'NONE',  ( 0.4862570985993235340, -5.003653737315397976, -12.97920246947884770 ) ) ;
#9694 = CARTESIAN_POINT ( 'NONE',  ( 0.000000000000000000, -1.732050807568877859, -1.752539433813135784E-17 ) ) ;
#9695 = LINE ( 'NONE', #6829, #2945 ) ;
#9696 = CARTESIAN_POINT ( 'NONE',  ( 1.342453679581834924, -5.476372339890114738, 13.74702459364882401 ) ) ;
#9697 = VERTEX_POINT ( 'NONE', #17290 ) ;
#9698 = ORIENTED_EDGE ( 'NONE', *, *, #6572, .F. ) ;
#9699 = ORIENTED_EDGE ( 'NONE', *, *, #13982, .F. ) ;
#9700 = ORIENTED_EDGE ( 'NONE', *, *, #11989, .F. ) ;
#9701 = CIRCLE ( 'NONE', #7271, 5.000000000000000888 ) ;
#9702 = LINE ( 'NONE', #10967, #11784 ) ;
#9703 = CARTESIAN_POINT ( 'NONE',  ( -5.923783695726434040, -7.499999999999999112, -16.97504159551249359 ) ) ;
#9704 = CARTESIAN_POINT ( 'NONE',  ( 16.56822296793089322, -0.006547366384936689071, -0.007741272030791150442 ) ) ;
#9705 = CARTESIAN_POINT ( 'NONE',  ( 16.57210152137263393, -0.01361613799508957709, 0.005118120558002058063 ) ) ;
#9706 = EDGE_CURVE ( 'NONE', #13879, #16287, #16353, .T. ) ;
#9707 = EDGE_CURVE ( 'NONE', #9813, #7378, #5238, .T. ) ;
#9708 = CARTESIAN_POINT ( 'NONE',  ( 16.56753206892534891, -0.008432171035096417550, 0.004368917149005420789 ) ) ;
#9709 = EDGE_CURVE ( 'NONE', #2485, #1319, #3814, .T. ) ;
#9710 = CARTESIAN_POINT ( 'NONE',  ( -53.40568638168567617, 9.314871387272406267, 6.000000000000000000 ) ) ;
#9711 = B_SPLINE_CURVE_WITH_KNOTS ( 'NONE', 3,
 ( #6475, #6665, #9149, #10880 ),
 .UNSPECIFIED., .F., .F.,
 ( 4, 4 ),
 ( 1.779952243785056044E-16, 0.002004993803842976610 ),
 .UNSPECIFIED. ) ;
#9712 = CARTESIAN_POINT ( 'NONE',  ( 2.123976203522053297, 10.37815841598508371, -11.67822624909914175 ) ) ;
#9713 = FACE_OUTER_BOUND ( 'NONE', #504, .T. ) ;
#9714 = ORIENTED_EDGE ( 'NONE', *, *, #14505, .T. ) ;
#9715 = ORIENTED_EDGE ( 'NONE', *, *, #3216, .T. ) ;
#9716 = EDGE_LOOP ( 'NONE', ( #10922, #17400, #1642, #11239 ) ) ;
#9717 =( BOUNDED_SURFACE ( )  B_SPLINE_SURFACE ( 3, 1, ( 
 ( #8447, #5296 ),
 ( #9967, #4149 ),
 ( #18757, #16961 ),
 ( #12834, #5654 ) ),
 .UNSPECIFIED., .F., .F., .T. ) 
 B_SPLINE_SURFACE_WITH_KNOTS ( ( 4, 4 ),
 ( 2, 2 ),
 ( 0.000000000000000000, 1.000000000000000000 ),
 ( 0.000000000000000000, 1.000000000000000000 ),
 .UNSPECIFIED. ) 
 GEOMETRIC_REPRESENTATION_ITEM ( )  RATIONAL_B_SPLINE_SURFACE ( (
 ( 1.000000000000000000, 1.000000000000000000),
 ( 0.9933953342250438912, 0.8357391271907739227),
 ( 0.9933953342250438912, 0.8357391271907739227),
 ( 1.000000000000000000, 1.000000000000000000) ) ) 
 REPRESENTATION_ITEM ( '' )  SURFACE ( )  );
#9718 = ORIENTED_EDGE ( 'NONE', *, *, #11215, .T. ) ;
#9719 = EDGE_CURVE ( 'NONE', #11500, #257, #14486, .T. ) ;
#9720 = CARTESIAN_POINT ( 'NONE',  ( 2.123976203522053297, 13.47898556379324297, -7.899625852120059299 ) ) ;
#9721 = FACE_OUTER_BOUND ( 'NONE', #14021, .T. ) ;
#9722 = DIRECTION ( 'NONE',  ( -1.000000000000000000, 0.000000000000000000, -0.000000000000000000 ) ) ;
#9723 = SURFACE_STYLE_USAGE ( .BOTH. , #12773 ) ;
#9724 = EDGE_LOOP ( 'NONE', ( #10698, #3246, #15938, #1590, #656, #262, #516, #8183, #4175, #6661, #14693, #1903, #3986, #17863, #15608, #4377 ) ) ;
#9725 = CARTESIAN_POINT ( 'NONE',  ( 1.861628059977344263, -0.5393144007391119654, 12.44564375541076728 ) ) ;
#9726 = CARTESIAN_POINT ( 'NONE',  ( 0.4862570985993235340, 11.67702470553376060, -7.559321496869298329 ) ) ;
#9727 = CARTESIAN_POINT ( 'NONE',  ( 6.538348415311011408, 2.499999999999998224, -12.00000000000000000 ) ) ;
#9728 = DIRECTION ( 'NONE',  ( -1.000000000000000000, 0.000000000000000000, 0.000000000000000000 ) ) ;
#9729 = CARTESIAN_POINT ( 'NONE',  ( 3.950837973638675393, -10.51028938476210328, -10.05648675950137871 ) ) ;
#9730 = DIRECTION ( 'NONE',  ( 1.000000000000000000, 0.000000000000000000, 0.000000000000000000 ) ) ;
#9731 = CARTESIAN_POINT ( 'NONE',  ( 0.3095370825347224519, -10.84046130709052491, -8.444334731364122604 ) ) ;
#9732 = CARTESIAN_POINT ( 'NONE',  ( 2.002547531651519996, 12.17374746633578475, 3.242439124566693476 ) ) ;
#9733 = ORIENTED_EDGE ( 'NONE', *, *, #5672, .T. ) ;
#9734 = ADVANCED_FACE ( 'NONE', ( #9934 ), #9896, .F. ) ;
#9736 = ORIENTED_EDGE ( 'NONE', *, *, #13998, .F. ) ;
#9735 = DIRECTION ( 'NONE',  ( 0.000000000000000000, 0.000000000000000000, 1.000000000000000000 ) ) ;
#9737 = AXIS2_PLACEMENT_3D ( 'NONE', #2301, #8327, #15663 ) ;
#9738 = DIRECTION ( 'NONE',  ( 1.000000000000000000, 0.000000000000000000, 0.000000000000000000 ) ) ;
#9739 = AXIS2_PLACEMENT_3D ( 'NONE', #4409, #17313, #4131 ) ;
#9740 = ADVANCED_FACE ( 'NONE', ( #8598 ), #6890, .T. ) ;
#9741 = VERTEX_POINT ( 'NONE', #1149 ) ;
#9742 = CARTESIAN_POINT ( 'NONE',  ( 1.846138399168762101, -4.238866729160323032, -11.69739621335926394 ) ) ;
#9743 = CARTESIAN_POINT ( 'NONE',  ( 0.000000000000000000, 0.000000000000000000, 7.000000000000000000 ) ) ;
#9744 = CARTESIAN_POINT ( 'NONE',  ( 2.002547531651519996, -12.17374746633575988, -3.242439124566779185 ) ) ;
#9745 = ORIENTED_EDGE ( 'NONE', *, *, #15026, .F. ) ;
#9746 = CARTESIAN_POINT ( 'NONE',  ( 0.4862570985993235340, 0.7479633556562450547, 13.89016912371017831 ) ) ;
#9747 = CARTESIAN_POINT ( 'NONE',  ( 1.560000000000000053, 0.000000000000000000, 2.999999999999998668 ) ) ;
#9748 = CARTESIAN_POINT ( 'NONE',  ( 3.074695600507260984, -10.75417554975707013, 11.23985886659431621 ) ) ;
#9749 = CARTESIAN_POINT ( 'NONE',  ( 0.000000000000000000, -1.732050807568877859, -1.752539433813135784E-17 ) ) ;
#9750 = DIRECTION ( 'NONE',  ( -1.000000000000000000, -0.000000000000000000, -0.000000000000000000 ) ) ;
#9751 = LINE ( 'NONE', #16929, #13841 ) ;
#9752 = DIRECTION ( 'NONE',  ( -1.000000000000000000, -0.000000000000000000, -0.000000000000000000 ) ) ;
#9754 = ORIENTED_EDGE ( 'NONE', *, *, #10921, .F. ) ;
#9753 = CARTESIAN_POINT ( 'NONE',  ( 0.000000000000000000, 0.000000000000000000, -3.000000000000000000 ) ) ;
#9755 = CARTESIAN_POINT ( 'NONE',  ( 0.4862570985993235340, 10.79774104611385965, -8.769551628660616771 ) ) ;
#9756 = LINE ( 'NONE', #14258, #9808 ) ;
#9757 = CARTESIAN_POINT ( 'NONE',  ( 1.977436885025011470, 11.52792723756289206, 10.21547824869447219 ) ) ;
#9758 = ADVANCED_FACE ( 'NONE', ( #2390 ), #6991, .F. ) ;
#9759 = ORIENTED_EDGE ( 'NONE', *, *, #11257, .T. ) ;
#9760 = CARTESIAN_POINT ( 'NONE',  ( -26.50000000000000711, -12.50000000000000178, 0.000000000000000000 ) ) ;
#9761 = CARTESIAN_POINT ( 'NONE',  ( 16.57778382496167424, 0.001819584982831899374, -0.01482878558584570412 ) ) ;
#9762 = ORIENTED_EDGE ( 'NONE', *, *, #9553, .F. ) ;
#9763 = CARTESIAN_POINT ( 'NONE',  ( 1.560000000000000053, -0.8660254037844384856, -1.500000000000000000 ) ) ;
#9764 = EDGE_CURVE ( 'NONE', #11032, #14416, #8510, .T. ) ;
#9765 = CARTESIAN_POINT ( 'NONE',  ( 1.846138399168762989, 10.30487220521570357, 6.971848976711047641 ) ) ;
#9766 = DIRECTION ( 'NONE',  ( -1.000000000000000000, -0.000000000000000000, -0.000000000000000000 ) ) ;
#9767 = CARTESIAN_POINT ( 'NONE',  ( 1.846138399168762101, -9.815003036200465658, 7.646096044339859787 ) ) ;
#9768 = UNCERTAINTY_MEASURE_WITH_UNIT (LENGTH_MEASURE( 1.000000000000000082E-05 ), #11310, 'distance_accuracy_value', 'NONE');
#9769 = APPLICATION_PROTOCOL_DEFINITION ( 'draft international standard', 'automotive_design', 1998, #4115 ) ;
#9770 = CARTESIAN_POINT ( 'NONE',  ( 0.000000000000000000, 0.8660254037844389297, -1.500000000000000000 ) ) ;
#9771 = CARTESIAN_POINT ( 'NONE',  ( 0.000000000000000000, 0.000000000000000000, -22.00000000000000000 ) ) ;
#9772 = CYLINDRICAL_SURFACE ( 'NONE', #17508, 2.499999999999992006 ) ;
#9773 = CARTESIAN_POINT ( 'NONE',  ( -5.000000000000000000, 20.00000000000000000, 8.000000000000000000 ) ) ;
#9774 = FACE_OUTER_BOUND ( 'NONE', #1143, .T. ) ;
#9775 = DIRECTION ( 'NONE',  ( 1.000000000000000000, 1.577021341797097560E-16, -0.000000000000000000 ) ) ;
#9776 = CARTESIAN_POINT ( 'NONE',  ( 1.562796894703937678, 0.000000000000000000, -12.15840553252917289 ) ) ;
#9777 = ORIENTED_EDGE ( 'NONE', *, *, #16792, .F. ) ;
#9778 = EDGE_CURVE ( 'NONE', #182, #9430, #13292, .T. ) ;
#9779 = ORIENTED_EDGE ( 'NONE', *, *, #16891, .F. ) ;
#9780 = VERTEX_POINT ( 'NONE', #7078 ) ;
#9781 = ORIENTED_EDGE ( 'NONE', *, *, #1397, .T. ) ;
#9782 = EDGE_CURVE ( 'NONE', #12560, #18215, #17894, .T. ) ;
#9783 = CARTESIAN_POINT ( 'NONE',  ( 6.000000000000000000, 20.00000000000000000, 4.000000000000000000 ) ) ;
#9784 =( BOUNDED_SURFACE ( )  B_SPLINE_SURFACE ( 3, 1, ( 
 ( #4995, #2854 ),
 ( #17306, #3937 ),
 ( #14153, #17399 ),
 ( #11217, #14438 ) ),
 .UNSPECIFIED., .F., .F., .T. ) 
 B_SPLINE_SURFACE_WITH_KNOTS ( ( 4, 4 ),
 ( 2, 2 ),
 ( 0.000000000000000000, 1.000000000000000000 ),
 ( 0.000000000000000000, 1.000000000000000000 ),
 .UNSPECIFIED. ) 
 GEOMETRIC_REPRESENTATION_ITEM ( )  RATIONAL_B_SPLINE_SURFACE ( (
 ( 1.000000000000000000, 1.000000000000000000),
 ( 0.9593108457356467333, 0.9995965569486454649),
 ( 0.9593108457356467333, 0.9995965569486454649),
 ( 1.000000000000000000, 1.000000000000000000) ) ) 
 REPRESENTATION_ITEM ( '' )  SURFACE ( )  );
#9785 = CARTESIAN_POINT ( 'NONE',  ( 0.000000000000000000, 0.000000000000000000, -12.00000000000000000 ) ) ;
#9786 = CARTESIAN_POINT ( 'NONE',  ( 8.438534575730034959, 5.415535776177522465, 4.221456476902686106 ) ) ;
#9787 = CARTESIAN_POINT ( 'NONE',  ( 3.950837973638676281, -6.316429227969383220, -13.10350451991847009 ) ) ;
#9788 = CARTESIAN_POINT ( 'NONE',  ( 2.750000000000000000, 5.817072295949927426E-16, -4.750000000000000000 ) ) ;
#9789 = CARTESIAN_POINT ( 'NONE',  ( 1.560000000000000053, 0.8660254037844389297, 1.500000000000000000 ) ) ;
#9790 = CARTESIAN_POINT ( 'NONE',  ( 1.342453679581834924, 0.9602753779832786662, -14.76648944001038188 ) ) ;
#9791 = CARTESIAN_POINT ( 'NONE',  ( 0.3058872367615226295, 12.87003593440628357, 4.821066432589371509 ) ) ;
#9792 = EDGE_LOOP ( 'NONE', ( #6589, #6471, #13504, #2973 ) ) ;
#9793 = ORIENTED_EDGE ( 'NONE', *, *, #6662, .T. ) ;
#9794 = ORIENTED_EDGE ( 'NONE', *, *, #5211, .F. ) ;
#9795 = EDGE_LOOP ( 'NONE', ( #11578, #5454, #7608, #2098, #4251 ) ) ;
#9796 = EDGE_CURVE ( 'NONE', #7766, #18684, #3925, .T. ) ;
#9797 = ADVANCED_FACE ( 'NONE', ( #15574 ), #2475, .T. ) ;
#9798 = LINE ( 'NONE', #15828, #1994 ) ;
#9799 = CARTESIAN_POINT ( 'NONE',  ( 1.560000000000000053, -1.732050807568877859, -1.752539433813135784E-17 ) ) ;
#9800 = CARTESIAN_POINT ( 'NONE',  ( 16.56753206892534891, 0.001549402974393146101, -0.009369540855502138735 ) ) ;
#9801 = CARTESIAN_POINT ( 'NONE',  ( 1.560000000000000053, 0.000000000000000000, 2.999999999999998668 ) ) ;
#9802 = CARTESIAN_POINT ( 'NONE',  ( 2.123976203522053297, -3.347755036805797779, -15.26039569100262838 ) ) ;
#9803 = ORIENTED_EDGE ( 'NONE', *, *, #17934, .T. ) ;
#9804 = CARTESIAN_POINT ( 'NONE',  ( 0.3095370825347234511, 8.444334731364163460, -10.84046130709049294 ) ) ;
#9805 = CARTESIAN_POINT ( 'NONE',  ( 1.845755665166725734, -11.97169564665393970, 3.386720041070682363 ) ) ;
#9806 = DIRECTION ( 'NONE',  ( 0.7561779333270775005, -0.2350349629540270657, 0.6106991889125030770 ) ) ;
#9807 = CARTESIAN_POINT ( 'NONE',  ( 0.3939822652208105902, 13.80035637018652395, 0.7002900021918435636 ) ) ;
#9808 = VECTOR ( 'NONE', #17598, 1000.000000000000000 ) ;
#9809 = CARTESIAN_POINT ( 'NONE',  ( 0.8740779401507027258, 13.83508928787419912, 3.609949156401401904 ) ) ;
#9810 = CARTESIAN_POINT ( 'NONE',  ( -30.00000000000000355, -12.50000000000000178, 6.000000000000000000 ) ) ;
#9811 = LINE ( 'NONE', #1311, #6460 ) ;
#9812 = CARTESIAN_POINT ( 'NONE',  ( 3.950837973638676281, -6.316429227969383220, -13.10350451991847009 ) ) ;
#9813 = VERTEX_POINT ( 'NONE', #13086 ) ;
#9815 = ORIENTED_EDGE ( 'NONE', *, *, #17435, .F. ) ;
#9814 = CARTESIAN_POINT ( 'NONE',  ( 16.56753206892534891, 0.004368917149004243779, -0.008432171035096398468 ) ) ;
#9816 = CARTESIAN_POINT ( 'NONE',  ( 0.3137051932979792457, -10.83767969834796929, -8.442169467526971616 ) ) ;
#9817 = VECTOR ( 'NONE', #5852, 1000.000000000000000 ) ;
#9818 = CARTESIAN_POINT ( 'NONE',  ( 0.3720661004400040439, -13.34435358167250207, -3.575426119359325750 ) ) ;
#9819 = ADVANCED_FACE ( 'NONE', ( #1435 ), #15166, .F. ) ;
#9820 = ADVANCED_FACE ( 'NONE', ( #10848 ), #709, .T. ) ;
#9821 = ORIENTED_EDGE ( 'NONE', *, *, #13673, .T. ) ;
#9822 = EDGE_CURVE ( 'NONE', #6216, #13188, #9322, .T. ) ;
#9823 = CARTESIAN_POINT ( 'NONE',  ( 3.512766787570980931, 13.55823433651926280, 6.535475144496921907 ) ) ;
#9824 = CARTESIAN_POINT ( 'NONE',  ( 1.846138399168762101, -12.43476674860266940, 0.4167076046095114505 ) ) ;
#9825 = DIRECTION ( 'NONE',  ( 0.000000000000000000, -0.000000000000000000, -1.000000000000000000 ) ) ;
#9826 = B_SPLINE_CURVE_WITH_KNOTS ( 'NONE', 3,
 ( #5272, #11116, #15499, #2399, #6809, #14068 ),
 .UNSPECIFIED., .F., .F.,
 ( 4, 2, 4 ),
 ( 0.000000000000000000, 0.0001828790815886940750, 0.0003657581631773881500 ),
 .UNSPECIFIED. ) ;
#9827 = DIRECTION ( 'NONE',  ( -1.000000000000000000, -0.000000000000000000, -0.000000000000000000 ) ) ;
#9828 = ORIENTED_EDGE ( 'NONE', *, *, #4942, .F. ) ;
#9829 = CARTESIAN_POINT ( 'NONE',  ( 4.336808689942017736E-15, -27.00000000000000000, 26.00000000000000000 ) ) ;
#9830 = CARTESIAN_POINT ( 'NONE',  ( 2.636624412714236865, 0.000000000000000000, 0.000000000000000000 ) ) ;
#9831 = B_SPLINE_CURVE_WITH_KNOTS ( 'NONE', 3,
 ( #6295, #4950, #12304, #6390 ),
 .UNSPECIFIED., .F., .F.,
 ( 4, 4 ),
 ( 1.734723475976807094E-17, 0.003005512676784844427 ),
 .UNSPECIFIED. ) ;
#9832 = DIRECTION ( 'NONE',  ( 0.000000000000000000, 0.000000000000000000, -1.000000000000000000 ) ) ;
#9833 = CARTESIAN_POINT ( 'NONE',  ( 2.636624412716062960, -2.161493821598612808, -15.91454522070331912 ) ) ;
#9834 = CARTESIAN_POINT ( 'NONE',  ( 3.686287386450715076E-15, -27.00000000000000000, 27.11316734529526329 ) ) ;
#9835 =( NAMED_UNIT ( * ) SI_UNIT ( $, .STERADIAN. ) SOLID_ANGLE_UNIT ( ) );
#9836 = LINE ( 'NONE', #2477, #9853 ) ;
#9837 = FACE_OUTER_BOUND ( 'NONE', #16690, .T. ) ;
#9839 = VERTEX_POINT ( 'NONE', #3570 ) ;
#9838 = CARTESIAN_POINT ( 'NONE',  ( 2.002547531651519996, -12.57989064830760206, 0.6781519942171299054 ) ) ;
#9840 = CARTESIAN_POINT ( 'NONE',  ( 0.3170788640506441158, -11.20690911610897800, -7.952793437297696499 ) ) ;
#9841 = CARTESIAN_POINT ( 'NONE',  ( 0.3142014840576535795, -12.94260032291125562, -4.608051180497059640 ) ) ;
#9842 = ORIENTED_EDGE ( 'NONE', *, *, #13607, .F. ) ;
#9843 = CARTESIAN_POINT ( 'NONE',  ( 1.845756295923361323, -9.776763338604659737, 7.694561132136919390 ) ) ;
#9844 = CARTESIAN_POINT ( 'NONE',  ( 1.918918678667074440, 12.49849921341423276, -0.6348738215465657975 ) ) ;
#9845 = B_SPLINE_CURVE_WITH_KNOTS ( 'NONE', 3,
 ( #6413, #2373, #7853, #12242 ),
 .UNSPECIFIED., .F., .F.,
 ( 4, 4 ),
 ( 7.039312503357838248E-16, 0.002004993803841917561 ),
 .UNSPECIFIED. ) ;
#9846 = ORIENTED_EDGE ( 'NONE', *, *, #11458, .F. ) ;
#9847 = DIRECTION ( 'NONE',  ( -1.000000000000000000, -0.000000000000000000, -0.000000000000000000 ) ) ;
#9848 = CARTESIAN_POINT ( 'NONE',  ( 1.342453679581834924, 0.9602753779832786662, -14.76648944001038188 ) ) ;
#9849 = EDGE_CURVE ( 'NONE', #14945, #8143, #5061, .T. ) ;
#9850 = LINE ( 'NONE', #17506, #6080 ) ;
#9851 = CARTESIAN_POINT ( 'NONE',  ( 2.002547531651519996, 7.942910686618313676, -9.778737580845612953 ) ) ;
#9852 = DIRECTION ( 'NONE',  ( -1.000000000000000000, 0.000000000000000000, 0.000000000000000000 ) ) ;
#9853 = VECTOR ( 'NONE', #1051, 1000.000000000000227 ) ;
#9854 = ORIENTED_EDGE ( 'NONE', *, *, #16963, .F. ) ;
#9855 = CONTEXT_DEPENDENT_SHAPE_REPRESENTATION ( #7571, #3417 ) ;
#9856 = CARTESIAN_POINT ( 'NONE',  ( 0.3058872367615226295, 0.6080468242582872662, -13.72992299905059177 ) ) ;
#9858 = ORIENTED_EDGE ( 'NONE', *, *, #13692, .F. ) ;
#9857 = CARTESIAN_POINT ( 'NONE',  ( 16.56822296793089322, 0.009385634690642057770, -0.003834730849371914118 ) ) ;
#9859 = CARTESIAN_POINT ( 'NONE',  ( 1.846613052777650976, 0.3401093050881815461, 12.43780859207239864 ) ) ;
#9860 = CARTESIAN_POINT ( 'NONE',  ( 1.846138399168762101, -0.4167076046094680408, -12.43476674860266940 ) ) ;
#9861 = DIRECTION ( 'NONE',  ( 0.000000000000000000, 0.000000000000000000, 1.000000000000000000 ) ) ;
#9862 = EDGE_CURVE ( 'NONE', #6378, #622, #1039, .T. ) ;
#9863 = EDGE_LOOP ( 'NONE', ( #11763, #1222, #18427, #16324, #6768, #14069 ) ) ;
#9864 = FACE_OUTER_BOUND ( 'NONE', #14553, .T. ) ;
#9865 = CARTESIAN_POINT ( 'NONE',  ( 1.846138399168762101, 6.971848976711159551, -10.30487220521562541 ) ) ;
#9866 = VERTEX_POINT ( 'NONE', #9744 ) ;
#9867 = ORIENTED_EDGE ( 'NONE', *, *, #8107, .T. ) ;
#9868 = AXIS2_PLACEMENT_3D ( 'NONE', #8949, #14776, #11919 ) ;
#9869 = EDGE_LOOP ( 'NONE', ( #3911, #9596 ) ) ;
#9870 = VECTOR ( 'NONE', #16904, 1000.000000000000000 ) ;
#9871 = ORIENTED_EDGE ( 'NONE', *, *, #13442, .T. ) ;
#9872 = CARTESIAN_POINT ( 'NONE',  ( 3.950837973638675393, -10.05648675950118509, -10.51028938476228980 ) ) ;
#9873 = EDGE_CURVE ( 'NONE', #381, #12288, #4009, .T. ) ;
#9874 = PRODUCT_DEFINITION_FORMATION_WITH_SPECIFIED_SOURCE ( 'ANY', '', #7708, .NOT_KNOWN. ) ;
#9875 = ORIENTED_EDGE ( 'NONE', *, *, #12678, .T. ) ;
#9876 = ADVANCED_FACE ( 'NONE', ( #12705 ), #11869, .F. ) ;
#9877 = EDGE_CURVE ( 'NONE', #10910, #14456, #12986, .T. ) ;
#9878 = CARTESIAN_POINT ( 'NONE',  ( 2.636624412715138366, -11.10302021257964888, 11.60464335004044223 ) ) ;
#9879 = CARTESIAN_POINT ( 'NONE',  ( 1.847380140988742703, -10.13114603776191380, -7.224522571381438496 ) ) ;
#9880 = PLANE ( 'NONE',  #2285 ) ;
#9881 = CARTESIAN_POINT ( 'NONE',  ( 2.320521194582656488, -7.743190876766163022, 13.71278319228045284 ) ) ;
#9882 = CARTESIAN_POINT ( 'NONE',  ( 0.3307726912345178572, 7.596084275799059427, -11.46720933246390572 ) ) ;
#9883 = AXIS2_PLACEMENT_3D ( 'NONE', #10021, #17103, #9825 ) ;
#9884 = CARTESIAN_POINT ( 'NONE',  ( 16.56872352241294521, -0.009382111268606286789, 0.004564908236400187953 ) ) ;
#9885 = MANIFOLD_SOLID_BREP ( 'M5 Clearance Hole1', #9071 ) ;
#9886 = B_SPLINE_CURVE_WITH_KNOTS ( 'NONE', 3,
 ( #2503, #16958, #8178, #3863, #12741, #9693 ),
 .UNSPECIFIED., .F., .F.,
 ( 4, 2, 4 ),
 ( 1.748223473168675632E-18, 0.0002017457492448088553, 0.0004034914984896159759 ),
 .UNSPECIFIED. ) ;
#9887 = CARTESIAN_POINT ( 'NONE',  ( 16.57778382496167424, 0.01306626476309378365, 0.007244066302947740205 ) ) ;
#9888 = CARTESIAN_POINT ( 'NONE',  ( 1.846138399168762101, 6.971848976711159551, -10.30487220521562541 ) ) ;
#9889 = EDGE_CURVE ( 'NONE', #349, #11883, #15489, .T. ) ;
#9890 = VERTEX_POINT ( 'NONE', #529 ) ;
#9891 = B_SPLINE_CURVE_WITH_KNOTS ( 'NONE', 3,
 ( #13243, #4459, #16215, #14676 ),
 .UNSPECIFIED., .F., .F.,
 ( 4, 4 ),
 ( 1.629624753548408703E-17, 0.003005512676784843126 ),
 .UNSPECIFIED. ) ;
#9892 = ORIENTED_EDGE ( 'NONE', *, *, #15265, .T. ) ;
#9893 = EDGE_CURVE ( 'NONE', #9212, #6154, #13794, .T. ) ;
#9894 = ORIENTED_EDGE ( 'NONE', *, *, #11552, .F. ) ;
#9895 = ORIENTED_EDGE ( 'NONE', *, *, #14449, .F. ) ;
#9896 =( BOUNDED_SURFACE ( )  B_SPLINE_SURFACE ( 3, 1, ( 
 ( #6797, #2751 ),
 ( #15762, #18443 ),
 ( #8414, #4212 ),
 ( #15863, #11201 ) ),
 .UNSPECIFIED., .F., .F., .T. ) 
 B_SPLINE_SURFACE_WITH_KNOTS ( ( 4, 4 ),
 ( 2, 2 ),
 ( 0.000000000000000000, 1.000000000000000000 ),
 ( 0.000000000000000000, 1.000000000000000000 ),
 .UNSPECIFIED. ) 
 GEOMETRIC_REPRESENTATION_ITEM ( )  RATIONAL_B_SPLINE_SURFACE ( (
 ( 1.000000000000000000, 1.000000000000000000),
 ( 0.7792777138730158093, 0.9689936506012928330),
 ( 0.7792777138730158093, 0.9689936506012928330),
 ( 1.000000000000000000, 1.000000000000000000) ) ) 
 REPRESENTATION_ITEM ( '' )  SURFACE ( )  );
#9897 = VECTOR ( 'NONE', #7534, 1000.000000000000000 ) ;
#9898 = CARTESIAN_POINT ( 'NONE',  ( 2.636624412714994037, -14.46769361191274328, -6.973567714907344950 ) ) ;
#9899 = CARTESIAN_POINT ( 'NONE',  ( 1.846138399168762101, -11.69739621335925328, 4.238866729160359448 ) ) ;
#9900 = B_SPLINE_CURVE_WITH_KNOTS ( 'NONE', 3,
 ( #8488, #2730, #6867, #14499 ),
 .UNSPECIFIED., .F., .F.,
 ( 4, 4 ),
 ( 0.000000000000000000, 0.002004993803842703825 ),
 .UNSPECIFIED. ) ;
#9901 = CARTESIAN_POINT ( 'NONE',  ( 3.950837973638668288, 0.000000000000000000, 0.000000000000000000 ) ) ;
#9902 = CARTESIAN_POINT ( 'NONE',  ( 1.846955891736119293, -7.098901504650428684, 10.21904526726843798 ) ) ;
#9903 = ORIENTED_EDGE ( 'NONE', *, *, #5699, .T. ) ;
#9904 = FACE_OUTER_BOUND ( 'NONE', #14674, .T. ) ;
#9905 = AXIS2_PLACEMENT_3D ( 'NONE', #8970, #13078, #13369 ) ;
#9906 = CARTESIAN_POINT ( 'NONE',  ( 0.4862570985993252548, -3.580942890621766406, 13.44146924561379741 ) ) ;
#9907 = CARTESIAN_POINT ( 'NONE',  ( 1.089171355198147673, 7.499999999999999112, -14.58290923294918606 ) ) ;
#9908 = CARTESIAN_POINT ( 'NONE',  ( -199.9999999999999716, 4.999999999999973355, 3.000000000000000000 ) ) ;
#9909 = CARTESIAN_POINT ( 'NONE',  ( 3.950837973638668288, 0.000000000000000000, 0.000000000000000000 ) ) ;
#9910 = CARTESIAN_POINT ( 'NONE',  ( 0.000000000000000000, 0.000000000000000000, 10.49999999999999822 ) ) ;
#9911 = FACE_OUTER_BOUND ( 'NONE', #10358, .T. ) ;
#9912 = CARTESIAN_POINT ( 'NONE',  ( 3.664313757352976708, 5.926151963190554817, -12.97355833021534011 ) ) ;
#9913 = ADVANCED_FACE ( 'NONE', ( #11196 ), #15725, .T. ) ;
#9914 = ORIENTED_EDGE ( 'NONE', *, *, #12637, .T. ) ;
#9915 = AXIS2_PLACEMENT_3D ( 'NONE', #10247, #2963, #1549 ) ;
#9916 = CIRCLE ( 'NONE', #6889, 16.06066017081991149 ) ;
#9918 = ORIENTED_EDGE ( 'NONE', *, *, #8668, .T. ) ;
#9917 = CARTESIAN_POINT ( 'NONE',  ( 25.00000000000000000, -7.500000000000000888, -22.00000000000000000 ) ) ;
#9919 = CARTESIAN_POINT ( 'NONE',  ( 2.636624412715999011, 2.161493821598055920, -15.91454522070273647 ) ) ;
#9920 = ORIENTED_EDGE ( 'NONE', *, *, #2704, .T. ) ;
#9921 = CARTESIAN_POINT ( 'NONE',  ( 0.3058872367615230181, -10.75034008168922206, 8.562166468153680654 ) ) ;
#9922 = ORIENTED_EDGE ( 'NONE', *, *, #14954, .T. ) ;
#9923 = CARTESIAN_POINT ( 'NONE',  ( 2.179449471770337432, -4.500000000000000000, -6.000000000000000000 ) ) ;
#9924 = DIRECTION ( 'NONE',  ( 0.000000000000000000, 0.000000000000000000, 1.000000000000000000 ) ) ;
#9925 = DIRECTION ( 'NONE',  ( -1.000000000000000000, 0.000000000000000000, 0.000000000000000000 ) ) ;
#9926 = DIRECTION ( 'NONE',  ( 1.540743955509788340E-33, 1.000000000000000000, 2.533398541561209262E-17 ) ) ;
#9927 = VERTEX_POINT ( 'NONE', #3969 ) ;
#9928 = DIRECTION ( 'NONE',  ( -0.000000000000000000, 1.000000000000000000, 1.224646799147353207E-16 ) ) ;
#9929 = CARTESIAN_POINT ( 'NONE',  ( 8.522092701127531811, -3.777034505568479528, -5.841710761610173108 ) ) ;
#9930 = B_SPLINE_CURVE_WITH_KNOTS ( 'NONE', 3,
 ( #2195, #9635, #9807, #14117, #17088, #8217 ),
 .UNSPECIFIED., .F., .F.,
 ( 4, 2, 4 ),
 ( 4.206917491929696500E-17, 0.0002014099069817281611, 0.0004028198139634142552 ),
 .UNSPECIFIED. ) ;
#9931 = AXIS2_PLACEMENT_3D ( 'NONE', #10173, #44, #8928 ) ;
#9932 = PLANE ( 'NONE',  #14970 ) ;
#9933 = AXIS2_PLACEMENT_3D ( 'NONE', #5058, #18251, #10997 ) ;
#9934 = FACE_OUTER_BOUND ( 'NONE', #12499, .T. ) ;
#9935 = DIRECTION ( 'NONE',  ( 0.000000000000000000, 0.000000000000000000, 1.000000000000000000 ) ) ;
#9936 = EDGE_CURVE ( 'NONE', #3961, #6426, #3407, .T. ) ;
#9937 =( LENGTH_UNIT ( ) NAMED_UNIT ( * ) SI_UNIT ( .MILLI., .METRE. ) );
#9938 = LINE ( 'NONE', #8513, #9564 ) ;
#9939 = EDGE_CURVE ( 'NONE', #3542, #14183, #15713, .T. ) ;
#9940 = EDGE_CURVE ( 'NONE', #13630, #10260, #12976, .T. ) ;
#9941 = CARTESIAN_POINT ( 'NONE',  ( 16.57210152137263393, -0.01453130299868639515, 0.0006600038696349324685 ) ) ;
#9943 = ORIENTED_EDGE ( 'NONE', *, *, #18008, .T. ) ;
#9942 = FACE_OUTER_BOUND ( 'NONE', #9792, .T. ) ;
#9944 = FACE_OUTER_BOUND ( 'NONE', #18210, .T. ) ;
#9945 = CIRCLE ( 'NONE', #13634, 5.000000000000000888 ) ;
#9946 = CARTESIAN_POINT ( 'NONE',  ( 2.636624412715137922, -14.46769361191291559, 6.973567714907789927 ) ) ;
#9947 = ORIENTED_EDGE ( 'NONE', *, *, #2704, .F. ) ;
#9948 = DIRECTION ( 'NONE',  ( -0.000000000000000000, -0.000000000000000000, 1.000000000000000000 ) ) ;
#9949 = CARTESIAN_POINT ( 'NONE',  ( 0.3939822652208145870, 10.75310269629521365, 8.678192463540208124 ) ) ;
#9950 = ORIENTED_EDGE ( 'NONE', *, *, #10896, .T. ) ;
#9951 = CARTESIAN_POINT ( 'NONE',  ( -32.49999999999999289, -12.50000000000000178, 0.000000000000000000 ) ) ;
#9952 = FILL_AREA_STYLE_COLOUR ( '', #8229 ) ;
#9953 = DIRECTION ( 'NONE',  ( 0.000000000000000000, 0.000000000000000000, 1.000000000000000000 ) ) ;
#9954 = DIRECTION ( 'NONE',  ( -0.000000000000000000, 0.000000000000000000, 1.000000000000000000 ) ) ;
#9955 = DIRECTION ( 'NONE',  ( 0.000000000000000000, 0.000000000000000000, 1.000000000000000000 ) ) ;
#9956 = ORIENTED_EDGE ( 'NONE', *, *, #3093, .F. ) ;
#9957 = STYLED_ITEM ( 'NONE', ( #5392 ), #16223 ) ;
#9958 = AXIS2_PLACEMENT_3D ( 'NONE', #16104, #14854, #6164 ) ;
#9959 =( NAMED_UNIT ( * ) SI_UNIT ( $, .STERADIAN. ) SOLID_ANGLE_UNIT ( ) );
#9960 = CARTESIAN_POINT ( 'NONE',  ( 1.845755665166724180, 7.694641135842960722, -9.776700214453546423 ) ) ;
#9961 = CARTESIAN_POINT ( 'NONE',  ( 0.3148213771069329203, -13.13560149728604109, 4.026433757158931925 ) ) ;
#9962 = CARTESIAN_POINT ( 'NONE',  ( 2.002547531651519996, 12.17374746633582561, -3.242439124566524278 ) ) ;
#9963 = ADVANCED_FACE ( 'NONE', ( #2616 ), #2346, .T. ) ;
#9964 =( REPRESENTATION_RELATIONSHIP ('NONE','NONE', #5200, #9113 ) REPRESENTATION_RELATIONSHIP_WITH_TRANSFORMATION ( #14081 )SHAPE_REPRESENTATION_RELATIONSHIP( ) );
#9965 = VERTEX_POINT ( 'NONE', #18582 ) ;
#9966 = CARTESIAN_POINT ( 'NONE',  ( 1.977228804422197062, -15.04020501276157518, -3.321884655131998265 ) ) ;
#9967 = CARTESIAN_POINT ( 'NONE',  ( 16.56822296793089322, 0.0007467251401288622394, -0.01011126603341004279 ) ) ;
#9968 = ORIENTED_EDGE ( 'NONE', *, *, #3408, .F. ) ;
#9969 = AXIS2_PLACEMENT_3D ( 'NONE', #6373, #6653, #9507 ) ;
#9970 = VECTOR ( 'NONE', #12650, 1000.000000000000000 ) ;
#9971 = ORIENTED_EDGE ( 'NONE', *, *, #12248, .F. ) ;
#9972 = CARTESIAN_POINT ( 'NONE',  ( 0.3095370825347224519, -8.444334731364081748, 10.84046130709055689 ) ) ;
#9973 = ORIENTED_EDGE ( 'NONE', *, *, #17326, .T. ) ;
#9974 = DIRECTION ( 'NONE',  ( 0.000000000000000000, 0.000000000000000000, 1.000000000000000000 ) ) ;
#9975 = CLOSED_SHELL ( 'NONE', ( #268, #5734, #5724, #3915, #15600, #10576, #976, #8191, #7640, #9103, #1869, #17348, #5924, #624, #12284, #11780, #18836, #3755, #8367, #3695, #5010, #3521, #15514, #8759, #8342, #18886, #17901, #13855, #1890, #18741, #4957, #11858, #10075 ) ) ;
#9976 = EDGE_LOOP ( 'NONE', ( #2844, #16762, #1421, #14525 ) ) ;
#9977 = EDGE_CURVE ( 'NONE', #10089, #10024, #15617, .T. ) ;
#9978 = CARTESIAN_POINT ( 'NONE',  ( 8.438534575730034959, -0.2320579683290609485, 6.862570336891074874 ) ) ;
#9979 = CARTESIAN_POINT ( 'NONE',  ( 0.3148208552358952583, 12.99355031785211168, -4.463611911212083783 ) ) ;
#9980 = CARTESIAN_POINT ( 'NONE',  ( 0.4754618798421162973, -0.7484603771385398563, 13.89949764182682301 ) ) ;
#9981 = DIRECTION ( 'NONE',  ( 0.000000000000000000, 0.000000000000000000, 1.000000000000000000 ) ) ;
#9982 = VECTOR ( 'NONE', #13404, 1000.000000000000114 ) ;
#9983 = CARTESIAN_POINT ( 'NONE',  ( 0.4862570985993235340, 7.559321496869593204, -11.67702470553357053 ) ) ;
#9984 = CARTESIAN_POINT ( 'NONE',  ( 0.3151928476913565258, -0.0002082997482820912163, -13.73922860838471927 ) ) ;
#9985 = EDGE_CURVE ( 'NONE', #3140, #18169, #8462, .T. ) ;
#9986 = CARTESIAN_POINT ( 'NONE',  ( 2.636624412715137922, -15.91454522070252153, 2.161493821597598508 ) ) ;
#9987 = EDGE_LOOP ( 'NONE', ( #18767, #14407, #16907, #1519, #11725, #10140, #6752, #15273, #12559, #7307, #8094, #840, #6793, #12909, #3445, #14720 ) ) ;
#9988 = ADVANCED_FACE ( 'NONE', ( #16974 ), #13816, .F. ) ;
#9989 = EDGE_CURVE ( 'NONE', #12131, #7670, #11174, .T. ) ;
#9990 = VERTEX_POINT ( 'NONE', #5404 ) ;
#9991 = CIRCLE ( 'NONE', #14889, 16.06066017081991149 ) ;
#9992 = VERTEX_POINT ( 'NONE', #15811 ) ;
#9993 = ORIENTED_EDGE ( 'NONE', *, *, #11617, .F. ) ;
#9994 = EDGE_LOOP ( 'NONE', ( #1390, #4075, #13526, #18120 ) ) ;
#9995 = DIRECTION ( 'NONE',  ( 0.000000000000000000, 1.000000000000000000, 0.000000000000000000 ) ) ;
#9996 = CARTESIAN_POINT ( 'NONE',  ( 16.56753206892534891, -0.001421777558676855365, -0.009389754735541546229 ) ) ;
#9997 = CARTESIAN_POINT ( 'NONE',  ( -20.00000000000000000, -2.500000000000000444, -22.00000000000000000 ) ) ;
#9998 = ORIENTED_EDGE ( 'NONE', *, *, #16515, .F. ) ;
#9999 = CARTESIAN_POINT ( 'NONE',  ( 2.320521194582183977, 6.542541239684722676, 14.32454473829914399 ) ) ;
#10000 = ADVANCED_FACE ( 'NONE', ( #11427 ), #18397, .T. ) ;
#10001 = CYLINDRICAL_SURFACE ( 'NONE', #6834, 2.499999999999995115 ) ;
#10002 = CARTESIAN_POINT ( 'NONE',  ( 2.482385025457376937, 7.499999999999866773, -13.17615586950464035 ) ) ;
#10003 = CARTESIAN_POINT ( 'NONE',  ( 0.3148208552358952028, -10.97826876274317875, 8.260375059853302560 ) ) ;
#10004 = CONICAL_SURFACE ( 'NONE', #1783, 14.54644660717763927, 0.8559913436420816257 ) ;
#10005 = PLANE ( 'NONE',  #179 ) ;
#10006 = CARTESIAN_POINT ( 'NONE',  ( -33.49999999999999289, -12.50000000000000178, -1.000000000000000000 ) ) ;
#10007 = CARTESIAN_POINT ( 'NONE',  ( 0.3720661004400040439, -7.524064345033547596, 11.58636699658212699 ) ) ;
#10008 = CARTESIAN_POINT ( 'NONE',  ( 1.847034903785829574, -4.063013886994788493, 11.76058231742743665 ) ) ;
#10009 = EDGE_LOOP ( 'NONE', ( #5611, #6849, #15919, #731 ) ) ;
#10011 = VECTOR ( 'NONE', #3371, 1000.000000000000000 ) ;
#10010 =( BOUNDED_SURFACE ( )  B_SPLINE_SURFACE ( 3, 1, ( 
 ( #3751, #15410 ),
 ( #9761, #7093 ),
 ( #8343, #11307 ),
 ( #15679, #13004 ) ),
 .UNSPECIFIED., .F., .F., .T. ) 
 B_SPLINE_SURFACE_WITH_KNOTS ( ( 4, 4 ),
 ( 2, 2 ),
 ( 0.000000000000000000, 1.000000000000000000 ),
 ( 0.000000000000000000, 1.000000000000000000 ),
 .UNSPECIFIED. ) 
 GEOMETRIC_REPRESENTATION_ITEM ( )  RATIONAL_B_SPLINE_SURFACE ( (
 ( 1.000000000000000000, 1.000000000000000000),
 ( 0.7792777138730158093, 0.9689936506012928330),
 ( 0.7792777138730158093, 0.9689936506012928330),
 ( 1.000000000000000000, 1.000000000000000000) ) ) 
 REPRESENTATION_ITEM ( '' )  SURFACE ( )  );
#10012 = ORIENTED_EDGE ( 'NONE', *, *, #14630, .F. ) ;
#10013 = DIRECTION ( 'NONE',  ( 0.000000000000000000, 0.000000000000000000, -1.000000000000000000 ) ) ;
#10014 = ORIENTED_EDGE ( 'NONE', *, *, #9134, .T. ) ;
#10015 = VERTEX_POINT ( 'NONE', #11152 ) ;
#10016 = DIRECTION ( 'NONE',  ( -1.000000000000000000, -0.000000000000000000, -0.000000000000000000 ) ) ;
#10017 = ADVANCED_FACE ( 'NONE', ( #12846 ), #4162, .T. ) ;
#10018 = ORIENTED_EDGE ( 'NONE', *, *, #17191, .F. ) ;
#10019 = CARTESIAN_POINT ( 'NONE',  ( 0.3137051932979792457, -12.91601973349266963, -4.679953077377624560 ) ) ;
#10020 = CARTESIAN_POINT ( 'NONE',  ( 1.560000000000000053, 0.000000000000000000, 0.000000000000000000 ) ) ;
#10021 = CARTESIAN_POINT ( 'NONE',  ( -199.9999999999999716, 9.999999999999973355, 6.000000000000000000 ) ) ;
#10022 = B_SPLINE_CURVE_WITH_KNOTS ( 'NONE', 3,
 ( #15579, #3738, #8333, #14251, #18273, #5451 ),
 .UNSPECIFIED., .F., .F.,
 ( 4, 2, 4 ),
 ( 2.710505431213761085E-19, 0.001657017934712013297, 0.003314035869424026594 ),
 .UNSPECIFIED. ) ;
#10023 = DIRECTION ( 'NONE',  ( 0.000000000000000000, 0.000000000000000000, 1.000000000000000000 ) ) ;
#10024 = VERTEX_POINT ( 'NONE', #2708 ) ;
#10025 = CARTESIAN_POINT ( 'NONE',  ( 2.369999999999999662, -4.750000000000000888, -5.817072295949926440E-16 ) ) ;
#10026 = ADVANCED_FACE ( 'NONE', ( #11060, #6666 ), #12479, .F. ) ;
#10027 = CARTESIAN_POINT ( 'NONE',  ( 0.3151928476913619104, -4.245853234426296474, -13.06671852871093265 ) ) ;
#10028 = CARTESIAN_POINT ( 'NONE',  ( 2.636624412714236865, 0.000000000000000000, 0.000000000000000000 ) ) ;
#10029 = CARTESIAN_POINT ( 'NONE',  ( 0.3137051932979792457, -13.20008686438103140, -3.805684345189927154 ) ) ;
#10030 = CARTESIAN_POINT ( 'NONE',  ( 0.3132635586635994507, -3.740017578711855695, 13.21855946425835882 ) ) ;
#10031 = CARTESIAN_POINT ( 'NONE',  ( 8.438534575730034959, -5.688336279099016402, -3.845978796786099885 ) ) ;
#10032 = DIRECTION ( 'NONE',  ( -0.9000142712801852962, 1.104208169119370286E-17, -0.4358604266184274434 ) ) ;
#10033 = DIRECTION ( 'NONE',  ( 1.335737076502141147E-14, 0.000000000000000000, -1.000000000000000000 ) ) ;
#10034 = CIRCLE ( 'NONE', #1812, 12.50000000000000355 ) ;
#10035 = CARTESIAN_POINT ( 'NONE',  ( 0.000000000000000000, 0.8660254037844389297, 1.500000000000000000 ) ) ;
#10037 = ORIENTED_EDGE ( 'NONE', *, *, #10814, .F. ) ;
#10036 = DIRECTION ( 'NONE',  ( 0.7561779333270775005, 0.6106991889125038542, 0.2350349629540249285 ) ) ;
#10038 = CARTESIAN_POINT ( 'NONE',  ( 5.000000000000006217, -30.00000000000000000, 26.00000000000000000 ) ) ;
#10039 = ORIENTED_EDGE ( 'NONE', *, *, #3886, .T. ) ;
#10040 = CARTESIAN_POINT ( 'NONE',  ( 2.179449471770337432, -4.500000000000000000, -3.000000000000000000 ) ) ;
#10041 = AXIS2_PLACEMENT_3D ( 'NONE', #8832, #5957, #17166 ) ;
#10042 = ORIENTED_EDGE ( 'NONE', *, *, #17360, .T. ) ;
#10043 = CARTESIAN_POINT ( 'NONE',  ( 1.847168016377981781, 10.17509564929258836, 7.161712042621497076 ) ) ;
#10044 = LINE ( 'NONE', #8426, #772 ) ;
#10045 = ORIENTED_EDGE ( 'NONE', *, *, #4878, .T. ) ;
#10046 = FACE_OUTER_BOUND ( 'NONE', #13005, .T. ) ;
#10047 = EDGE_CURVE ( 'NONE', #12518, #11575, #11148, .T. ) ;
#10048 = EDGE_CURVE ( 'NONE', #14890, #10634, #3082, .T. ) ;
#10049 = EDGE_CURVE ( 'NONE', #17236, #2621, #16200, .T. ) ;
#10050 = CARTESIAN_POINT ( 'NONE',  ( -199.9999999999999716, -40.00000000000003553, 3.000000000000000000 ) ) ;
#10051 = VECTOR ( 'NONE', #18619, 1000.000000000000000 ) ;
#10052 = CARTESIAN_POINT ( 'NONE',  ( 1.847034903785818694, -9.929438108952092890, -7.498375632854726192 ) ) ;
#10053 = AXIS2_PLACEMENT_3D ( 'NONE', #4498, #4590, #13467 ) ;
#10054 = FACE_BOUND ( 'NONE', #8277, .T. ) ;
#10055 = LINE ( 'NONE', #8262, #13016 ) ;
#10056 = ORIENTED_EDGE ( 'NONE', *, *, #6707, .T. ) ;
#10057 = B_SPLINE_CURVE_WITH_KNOTS ( 'NONE', 3,
 ( #3746, #12266, #16754, #6352, #10650, #3659 ),
 .UNSPECIFIED., .F., .F.,
 ( 4, 2, 4 ),
 ( 3.229102830436655475E-17, 0.0001825746017570572058, 0.0003651492035140821565 ),
 .UNSPECIFIED. ) ;
#10059 = ORIENTED_EDGE ( 'NONE', *, *, #15270, .F. ) ;
#10058 = CARTESIAN_POINT ( 'NONE',  ( 16.57210152137263393, 0.009075239946109033701, 0.01136813053532163831 ) ) ;
#10060 = B_SPLINE_CURVE_WITH_KNOTS ( 'NONE', 3,
 ( #18203, #5110, #15329, #9416, #13801, #1967 ),
 .UNSPECIFIED., .F., .F.,
 ( 4, 2, 4 ),
 ( 0.000000000000000000, 0.0001828790815886950779, 0.0003657581631773901558 ),
 .UNSPECIFIED. ) ;
#10061 = CARTESIAN_POINT ( 'NONE',  ( 2.002547531651519996, 0.6781519942171739812, 12.57989064830759851 ) ) ;
#10062 = CARTESIAN_POINT ( 'NONE',  ( 1.847247051441592625, 3.685275815977189673, 11.88474976472813971 ) ) ;
#10063 = PLANE ( 'NONE',  #18530 ) ;
#10064 = ORIENTED_EDGE ( 'NONE', *, *, #2226, .F. ) ;
#10065 = DIRECTION ( 'NONE',  ( 0.000000000000000000, -0.000000000000000000, 1.000000000000000000 ) ) ;
#10066 = CARTESIAN_POINT ( 'NONE',  ( 1.845756295923360435, -7.694561132136879422, -9.776763338604684606 ) ) ;
#10067 = ORIENTED_EDGE ( 'NONE', *, *, #9239, .F. ) ;
#10068 = ORIENTED_EDGE ( 'NONE', *, *, #14338, .F. ) ;
#10069 = DIRECTION ( 'NONE',  ( 0.000000000000000000, 0.000000000000000000, -1.000000000000000000 ) ) ;
#10070 = EDGE_LOOP ( 'NONE', ( #1101, #17454 ) ) ;
#10071 = CARTESIAN_POINT ( 'NONE',  ( 12.00000000000000711, -15.99999999999999645, 7.000000000000000000 ) ) ;
#10072 = EDGE_CURVE ( 'NONE', #400, #8123, #12943, .T. ) ;
#10073 = ORIENTED_EDGE ( 'NONE', *, *, #7389, .F. ) ;
#10074 = LINE ( 'NONE', #5762, #16678 ) ;
#10075 = ADVANCED_FACE ( 'NONE', ( #8745 ), #5647, .F. ) ;
#10076 = CARTESIAN_POINT ( 'NONE',  ( 1.846955891736119071, -10.21904526726841311, -7.098901504650468652 ) ) ;
#10077 = ADVANCED_FACE ( 'NONE', ( #17533 ), #17737, .F. ) ;
#10078 = CARTESIAN_POINT ( 'NONE',  ( 1.959283090834839314, 9.750336807931262229, -7.909254450748897547 ) ) ;
#10079 = FACE_OUTER_BOUND ( 'NONE', #8702, .T. ) ;
#10080 = CIRCLE ( 'NONE', #13399, 7.000000000000000000 ) ;
#10081 = SURFACE_STYLE_FILL_AREA ( #17065 ) ;
#10082 = CARTESIAN_POINT ( 'NONE',  ( 16.57778382496167424, -0.001819584982832002807, 0.01482878558584568851 ) ) ;
#10083 = CARTESIAN_POINT ( 'NONE',  ( 1.959283090834842200, 10.53516775895160507, 6.829027319138286423 ) ) ;
#10084 = CARTESIAN_POINT ( 'NONE',  ( 0.3095370825347224519, 11.38092634279639626, -7.700448427571749299 ) ) ;
#10085 = CARTESIAN_POINT ( 'NONE',  ( 16.58200780006414732, 0.01080144354108870768, 0.002844973367391462511 ) ) ;
#10086 = VERTEX_POINT ( 'NONE', #1485 ) ;
#10087 = ORIENTED_EDGE ( 'NONE', *, *, #5973, .F. ) ;
#10088 = EDGE_LOOP ( 'NONE', ( #17084, #1086 ) ) ;
#10089 = VERTEX_POINT ( 'NONE', #7514 ) ;
#10090 = ORIENTED_EDGE ( 'NONE', *, *, #5975, .T. ) ;
#10091 = DIRECTION ( 'NONE',  ( 0.7561779333270775005, -0.3559159372837316093, -0.5491072561318351974 ) ) ;
#10092 = CARTESIAN_POINT ( 'NONE',  ( -20.00000000000000000, 2.499999999999998668, -17.00000000000000000 ) ) ;
#10093 = B_SPLINE_CURVE_WITH_KNOTS ( 'NONE', 3,
 ( #16730, #6692, #13941, #2374 ),
 .UNSPECIFIED., .F., .F.,
 ( 4, 4 ),
 ( 3.727890075251872641E-16, 0.002004993803842877297 ),
 .UNSPECIFIED. ) ;
#10094 = CARTESIAN_POINT ( 'NONE',  ( -32.49999999999999289, -12.50000000000000178, 6.000000000000000000 ) ) ;
#10095 = VERTEX_POINT ( 'NONE', #14377 ) ;
#10096 = DIRECTION ( 'NONE',  ( 1.000000000000000000, 0.000000000000000000, 0.000000000000000000 ) ) ;
#10097 = EDGE_CURVE ( 'NONE', #11870, #5180, #17524, .T. ) ;
#10098 = CARTESIAN_POINT ( 'NONE',  ( 2.636624412716062960, 6.973567714909310489, -14.46769361191320868 ) ) ;
#10099 = CIRCLE ( 'NONE', #5222, 2.500000000000000000 ) ;
#10100 = EDGE_CURVE ( 'NONE', #16664, #13997, #17061, .T. ) ;
#10101 = CARTESIAN_POINT ( 'NONE',  ( 0.9342146476565840185, 7.500000000000134115, -13.05973490260135073 ) ) ;
#10102 = DIRECTION ( 'NONE',  ( -0.000000000000000000, -0.000000000000000000, -1.000000000000000000 ) ) ;
#10103 = CARTESIAN_POINT ( 'NONE',  ( 2.636624412716062960, -2.161493821598612808, -15.91454522070331912 ) ) ;
#10104 = B_SPLINE_CURVE_WITH_KNOTS ( 'NONE', 3,
 ( #5444, #9560, #11102, #15661 ),
 .UNSPECIFIED., .F., .F.,
 ( 4, 4 ),
 ( 1.914591753770035818E-17, 0.002004993803842692549 ),
 .UNSPECIFIED. ) ;
#10105 = DIRECTION ( 'NONE',  ( -1.000000000000000000, 0.000000000000000000, -0.000000000000000000 ) ) ;
#10106 = CARTESIAN_POINT ( 'NONE',  ( 1.847034903785824023, 3.625649561595307269, 11.90269060117935496 ) ) ;
#10107 = CARTESIAN_POINT ( 'NONE',  ( 0.3170788640506440603, -11.02668139258435787, -8.200855617524654306 ) ) ;
#10108 = DIRECTION ( 'NONE',  ( 0.000000000000000000, 0.000000000000000000, 1.000000000000000000 ) ) ;
#10109 = VERTEX_POINT ( 'NONE', #13230 ) ;
#10110 = PRODUCT_DEFINITION_SHAPE ( 'NONE', 'NONE',  #18907 ) ;
#10111 =( REPRESENTATION_RELATIONSHIP ('NONE','NONE', #5200, #14244 ) REPRESENTATION_RELATIONSHIP_WITH_TRANSFORMATION ( #16077 )SHAPE_REPRESENTATION_RELATIONSHIP( ) );
#10112 = EDGE_LOOP ( 'NONE', ( #15272, #6833, #17966, #15582 ) ) ;
#10113 = ORIENTED_EDGE ( 'NONE', *, *, #5855, .F. ) ;
#10114 = TOROIDAL_SURFACE ( 'NONE', #12851, 3.499999999999994671, 0.5000000000000000000 ) ;
#10115 = EDGE_CURVE ( 'NONE', #9334, #4587, #4440, .T. ) ;
#10116 = ORIENTED_EDGE ( 'NONE', *, *, #5321, .F. ) ;
#10117 = CARTESIAN_POINT ( 'NONE',  ( 2.002547531651521773, 9.778737580845699995, 7.942910686618207983 ) ) ;
#10118 = ORIENTED_EDGE ( 'NONE', *, *, #11526, .T. ) ;
#10119 = FACE_BOUND ( 'NONE', #187, .T. ) ;
#10120 = CARTESIAN_POINT ( 'NONE',  ( 2.353870697619111496, -8.216087327473003299, 10.00946331859660710 ) ) ;
#10121 = LINE ( 'NONE', #7363, #12331 ) ;
#10122 = LINE ( 'NONE', #15946, #16947 ) ;
#10123 = VERTEX_POINT ( 'NONE', #2891 ) ;
#10124 = PLANE ( 'NONE',  #4113 ) ;
#10125 = CARTESIAN_POINT ( 'NONE',  ( -4.999999999999995559, -27.00000000000000000, 6.000000000000000000 ) ) ;
#10126 = CARTESIAN_POINT ( 'NONE',  ( 0.3151930723728451622, -13.73922999529477451, -0.07645105377001075453 ) ) ;
#10127 = DIRECTION ( 'NONE',  ( 1.000000000000000000, 0.000000000000000000, 0.000000000000000000 ) ) ;
#10128 = CARTESIAN_POINT ( 'NONE',  ( 0.4862570985993235340, -8.769551628660812170, 10.79774104611370333 ) ) ;
#10129 = CARTESIAN_POINT ( 'NONE',  ( -1.500000000000000888, 4.769696007084728073, 5.000000000000000000 ) ) ;
#10130 = DIRECTION ( 'NONE',  ( 1.826842780715651273E-15, -2.870007559987786327E-17, 1.000000000000000000 ) ) ;
#10131 = ADVANCED_FACE ( 'NONE', ( #4442 ), #14756, .T. ) ;
#10132 = DIRECTION ( 'NONE',  ( -1.000000000000000000, -0.000000000000000000, -0.000000000000000000 ) ) ;
#10133 = ORIENTED_EDGE ( 'NONE', *, *, #6707, .F. ) ;
#10134 = VECTOR ( 'NONE', #16534, 1000.000000000000000 ) ;
#10135 = LINE ( 'NONE', #7184, #6771 ) ;
#10137 = VERTEX_POINT ( 'NONE', #1575 ) ;
#10136 = CARTESIAN_POINT ( 'NONE',  ( 1.847372867223026738, 0.1054171785008226614, -12.44269075185938433 ) ) ;
#10138 = CARTESIAN_POINT ( 'NONE',  ( 0.000000000000000000, 0.000000000000000000, 4.750000000000000000 ) ) ;
#10139 = CARTESIAN_POINT ( 'NONE',  ( 2.002547531651519996, -10.57595306287287329, -6.845637710436306200 ) ) ;
#10140 = ORIENTED_EDGE ( 'NONE', *, *, #11103, .T. ) ;
#10141 = ADVANCED_FACE ( 'NONE', ( #16108 ), #1362, .F. ) ;
#10142 = CARTESIAN_POINT ( 'NONE',  ( 0.3142014840576516921, 4.608051180497103161, -12.94260032291123785 ) ) ;
#10143 = CARTESIAN_POINT ( 'NONE',  ( 4.755015822784811164, -4.336808689942017736E-16, 0.000000000000000000 ) ) ;
#10144 = ORIENTED_EDGE ( 'NONE', *, *, #17142, .T. ) ;
#10145 = CARTESIAN_POINT ( 'NONE',  ( 0.3058872367615226295, 7.578326039752606214, 11.46514199369360298 ) ) ;
#10146 = CARTESIAN_POINT ( 'NONE',  ( 16.57210152137263393, 0.01361613799508961699, -0.005118120558001958316 ) ) ;
#10147 = CARTESIAN_POINT ( 'NONE',  ( 0.3148213771069381384, -4.463459503829087183, 12.99360322443201277 ) ) ;
#10148 = CARTESIAN_POINT ( 'NONE',  ( 0.4385251269669942498, 11.63205320541534071, -7.540955776459614235 ) ) ;
#10149 = EDGE_LOOP ( 'NONE', ( #18765, #11519, #17077, #9428 ) ) ;
#10150 = ITEM_DEFINED_TRANSFORMATION ( 'NONE', 'NONE', #15463,  #2030 ) ;
#10151 = AXIS2_PLACEMENT_3D ( 'NONE', #4165, #2798, #17738 ) ;
#10152 = FACE_OUTER_BOUND ( 'NONE', #5552, .T. ) ;
#10153 = CARTESIAN_POINT ( 'NONE',  ( 0.4754618798421171855, 13.89949764182682657, -0.7484603771384882309 ) ) ;
#10154 = ADVANCED_FACE ( 'NONE', ( #10079 ), #12476, .F. ) ;
#10155 = CARTESIAN_POINT ( 'NONE',  ( 0.4754618798421171855, -13.45049478164057000, -3.583352865732813530 ) ) ;
#10156 = DIRECTION ( 'NONE',  ( 1.000000000000000000, 0.000000000000000000, 0.000000000000000000 ) ) ;
#10157 = CARTESIAN_POINT ( 'NONE',  ( 1.342453679581834924, 14.34050741580211508, -3.649820028552582585 ) ) ;
#10158 = EDGE_CURVE ( 'NONE', #1652, #13434, #7614, .T. ) ;
#10159 = ORIENTED_EDGE ( 'NONE', *, *, #15741, .T. ) ;
#10160 = CARTESIAN_POINT ( 'NONE',  ( 2.002547531651519996, -9.778737580845639599, -7.942910686618280813 ) ) ;
#10161 = CARTESIAN_POINT ( 'NONE',  ( 0.3095370825347224519, 4.681152801286160070, 12.91933430393609861 ) ) ;
#10162 = ORIENTED_EDGE ( 'NONE', *, *, #17675, .F. ) ;
#10163 = EDGE_LOOP ( 'NONE', ( #13075, #11345, #14901, #2525 ) ) ;
#10164 = B_SPLINE_CURVE_WITH_KNOTS ( 'NONE', 3,
 ( #13601, #519, #2313, #2223, #3658, #9299 ),
 .UNSPECIFIED., .F., .F.,
 ( 4, 2, 4 ),
 ( 0.000000000000000000, 0.001500839035891550922, 0.003001678071783101844 ),
 .UNSPECIFIED. ) ;
#10165 = DIRECTION ( 'NONE',  ( -1.000000000000000000, 0.000000000000000000, 0.000000000000000000 ) ) ;
#10166 = ORIENTED_EDGE ( 'NONE', *, *, #6712, .T. ) ;
#10167 = CARTESIAN_POINT ( 'NONE',  ( 3.950837973638668288, 0.000000000000000000, 0.000000000000000000 ) ) ;
#10168 = VERTEX_POINT ( 'NONE', #18021 ) ;
#10169 = VECTOR ( 'NONE', #2262, 1000.000000000000000 ) ;
#10170 = DIRECTION ( 'NONE',  ( -0.000000000000000000, 0.5000000000000004441, 0.8660254037844383745 ) ) ;
#10171 = CARTESIAN_POINT ( 'NONE',  ( 16.56822296793089322, 0.01011126603341077484, -0.0007467251401297481410 ) ) ;
#10172 = DIRECTION ( 'NONE',  ( 0.000000000000000000, 0.000000000000000000, 1.000000000000000000 ) ) ;
#10173 = CARTESIAN_POINT ( 'NONE',  ( 4.000000000000000000, 20.00000000000000000, 7.000000000000000000 ) ) ;
#10174 = CARTESIAN_POINT ( 'NONE',  ( 2.123976203522053741, -15.54801196254788209, 1.531817366691698545 ) ) ;
#10175 = CARTESIAN_POINT ( 'NONE',  ( -199.9999999999999716, 0.000000000000000000, -2.000000000000000000 ) ) ;
#10176 = CARTESIAN_POINT ( 'NONE',  ( 0.3137051932979757485, -8.442169467526770887, -10.83767969834812561 ) ) ;
#10177 = CARTESIAN_POINT ( 'NONE',  ( 0.3137051932979792457, -7.698472063774386420, -11.37800749014139612 ) ) ;
#10178 = AXIS2_PLACEMENT_3D ( 'NONE', #100, #8883, #10033 ) ;
#10179 = EDGE_CURVE ( 'NONE', #16693, #10980, #1394, .T. ) ;
#10180 = ORIENTED_EDGE ( 'NONE', *, *, #14874, .T. ) ;
#10181 = ADVANCED_FACE ( 'NONE', ( #13799 ), #8708, .T. ) ;
#10182 = AXIS2_PLACEMENT_3D ( 'NONE', #17975, #4877, #11175 ) ;
#10183 = ORIENTED_EDGE ( 'NONE', *, *, #4315, .T. ) ;
#10184 = ORIENTED_EDGE ( 'NONE', *, *, #9719, .F. ) ;
#10185 = ORIENTED_EDGE ( 'NONE', *, *, #12688, .F. ) ;
#10186 = VERTEX_POINT ( 'NONE', #1871 ) ;
#10187 = CARTESIAN_POINT ( 'NONE',  ( 1.846524061778021419, 4.180439405448487911, -11.71897913237544664 ) ) ;
#10188 = DIRECTION ( 'NONE',  ( 0.000000000000000000, -1.000000000000000000, 0.000000000000000000 ) ) ;
#10189 = CARTESIAN_POINT ( 'NONE',  ( 0.4862570985993235340, 8.769551628660890330, -10.79774104611363761 ) ) ;
#10190 = ORIENTED_EDGE ( 'NONE', *, *, #12726, .T. ) ;
#10191 = DIRECTION ( 'NONE',  ( 1.000000000000000000, 0.000000000000000000, 0.000000000000000000 ) ) ;
#10192 = CARTESIAN_POINT ( 'NONE',  ( 2.747332970342022840, -2.409922051470793747, 16.17136872824897864 ) ) ;
#10193 = AXIS2_PLACEMENT_3D ( 'NONE', #5787, #1210, #17460 ) ;
#10194 = DIRECTION ( 'NONE',  ( 0.000000000000000000, 0.000000000000000000, 1.000000000000000000 ) ) ;
#10195 = FACE_OUTER_BOUND ( 'NONE', #9795, .T. ) ;
#10196 = CARTESIAN_POINT ( 'NONE',  ( 0.000000000000000000, -0.8660254037844384856, 1.500000000000000000 ) ) ;
#10197 = CARTESIAN_POINT ( 'NONE',  ( 2.747332970342022840, 14.49942876448603180, -7.555624153089486761 ) ) ;
#10198 = CARTESIAN_POINT ( 'NONE',  ( -30.00000000000000355, -12.50000000000000178, -1.000000000000000000 ) ) ;
#10199 = CARTESIAN_POINT ( 'NONE',  ( 16.56782317627811096, 0.003357783021327817585, 0.009228812961908668469 ) ) ;
#10200 = CARTESIAN_POINT ( 'NONE',  ( 20.00000000000000711, -45.00000000000000000, 3.000000000000000000 ) ) ;
#10201 = CARTESIAN_POINT ( 'NONE',  ( -194.9999999999999716, -10.00000000000002665, 3.000000000000000000 ) ) ;
#10202 = VERTEX_POINT ( 'NONE', #9319 ) ;
#10203 = EDGE_LOOP ( 'NONE', ( #17519, #2982, #7161, #2471 ) ) ;
#10204 = AXIS2_PLACEMENT_3D ( 'NONE', #4657, #15066, #4563 ) ;
#10205 = ORIENTED_EDGE ( 'NONE', *, *, #18181, .F. ) ;
#10206 = EDGE_CURVE ( 'NONE', #14287, #11172, #630, .T. ) ;
#10207 = ORIENTED_EDGE ( 'NONE', *, *, #3630, .T. ) ;
#10208 = CARTESIAN_POINT ( 'NONE',  ( 1.846138399168762989, 9.815003036200414144, 7.646096044339929954 ) ) ;
#10209 = EDGE_CURVE ( 'NONE', #13548, #16346, #9031, .T. ) ;
#10210 = AXIS2_PLACEMENT_3D ( 'NONE', #13106, #5733, #13194 ) ;
#10211 = EDGE_LOOP ( 'NONE', ( #7935, #8052, #1763, #12431 ) ) ;
#10212 = DIRECTION ( 'NONE',  ( -1.000000000000000000, 0.000000000000000000, 0.000000000000000000 ) ) ;
#10213 = AXIS2_PLACEMENT_3D ( 'NONE', #3322, #376, #13553 ) ;
#10214 = CARTESIAN_POINT ( 'NONE',  ( 1.846138399168762101, 11.95493567637855392, -3.446241763652874379 ) ) ;
#10215 = CARTESIAN_POINT ( 'NONE',  ( 1.342453679581834924, 12.51077660954477189, -7.902645620902311485 ) ) ;
#10216 = ORIENTED_EDGE ( 'NONE', *, *, #3988, .T. ) ;
#10217 = DIRECTION ( 'NONE',  ( 0.000000000000000000, -1.000000000000000000, 0.000000000000000000 ) ) ;
#10218 = EDGE_CURVE ( 'NONE', #9992, #5117, #9621, .T. ) ;
#10219 = DIRECTION ( 'NONE',  ( -0.7561779333270775005, 0.03481510524964793324, 0.6534392409364820908 ) ) ;
#10220 = CARTESIAN_POINT ( 'NONE',  ( -20.00000000000000000, -7.500000000000000888, -17.00000000000000000 ) ) ;
#10221 =( BOUNDED_SURFACE ( )  B_SPLINE_SURFACE ( 3, 1, ( 
 ( #17232, #4247 ),
 ( #11238, #9696 ),
 ( #11138, #3870 ),
 ( #15701, #17140 ) ),
 .UNSPECIFIED., .F., .F., .T. ) 
 B_SPLINE_SURFACE_WITH_KNOTS ( ( 4, 4 ),
 ( 2, 2 ),
 ( 0.000000000000000000, 1.000000000000000000 ),
 ( 0.000000000000000000, 1.000000000000000000 ),
 .UNSPECIFIED. ) 
 GEOMETRIC_REPRESENTATION_ITEM ( )  RATIONAL_B_SPLINE_SURFACE ( (
 ( 1.000000000000000000, 1.000000000000000000),
 ( 0.7792777138730160313, 0.9689936506012927220),
 ( 0.7792777138730160313, 0.9689936506012927220),
 ( 1.000000000000000000, 1.000000000000000000) ) ) 
 REPRESENTATION_ITEM ( '' )  SURFACE ( )  );
#10222 = CARTESIAN_POINT ( 'NONE',  ( 1.846524061778021419, 11.71897913237549105, 4.180439405448364454 ) ) ;
#10223 = LINE ( 'NONE', #194, #18136 ) ;
#10224 = AXIS2_PLACEMENT_3D ( 'NONE', #12546, #18377, #13712 ) ;
#10225 = AXIS2_PLACEMENT_3D ( 'NONE', #9127, #6715, #6366 ) ;
#10226 = AXIS2_PLACEMENT_3D ( 'NONE', #10384, #14677, #4179 ) ;
#10227 = DIRECTION ( 'NONE',  ( -0.000000000000000000, 1.000000000000000000, -0.000000000000000000 ) ) ;
#10228 = ORIENTED_EDGE ( 'NONE', *, *, #4112, .T. ) ;
#10229 = PRODUCT_DEFINITION ( 'UNKNOWN', '', #8077, #7728 ) ;
#10230 = EDGE_CURVE ( 'NONE', #10313, #2807, #7906, .T. ) ;
#10231 = CARTESIAN_POINT ( 'NONE',  ( 3.512766787570793969, 2.682019731918377836, 14.81029789862155255 ) ) ;
#10233 = ORIENTED_EDGE ( 'NONE', *, *, #1458, .T. ) ;
#10232 = CARTESIAN_POINT ( 'NONE',  ( 0.8740779401507798863, 5.211551231203803702, 13.31469722824348878 ) ) ;
#10234 = CARTESIAN_POINT ( 'NONE',  ( 16.56753206892534891, -0.006760771273035160941, 0.006669401563385170262 ) ) ;
#10235 = ADVANCED_FACE ( 'NONE', ( #15148 ), #2688, .F. ) ;
#10236 = ADVANCED_FACE ( 'NONE', ( #9033 ), #1997, .F. ) ;
#10237 = CARTESIAN_POINT ( 'NONE',  ( 8.438534575730034959, 3.845978796786037268, 5.688336279099058146 ) ) ;
#10238 = ORIENTED_EDGE ( 'NONE', *, *, #1804, .F. ) ;
#10239 = CARTESIAN_POINT ( 'NONE',  ( 1.847372867223027404, 10.00438561114523850, 7.398914411685026060 ) ) ;
#10240 = VECTOR ( 'NONE', #5351, 1000.000000000000227 ) ;
#10241 = CARTESIAN_POINT ( 'NONE',  ( 5.052632128771786135, -7.500000000000000888, -16.81774875490144794 ) ) ;
#10242 = VECTOR ( 'NONE', #15838, 1000.000000000000000 ) ;
#10243 = VERTEX_POINT ( 'NONE', #338 ) ;
#10244 = DIRECTION ( 'NONE',  ( 0.000000000000000000, 0.8660254037844384856, -0.5000000000000004441 ) ) ;
#10245 = CARTESIAN_POINT ( 'NONE',  ( 1.254009781011619529, -3.563484327698362542, 14.24044713813325558 ) ) ;
#10246 = DIRECTION ( 'NONE',  ( -0.7635533937278216055, -0.02138673900301441000, -0.6453904417649389824 ) ) ;
#10247 = CARTESIAN_POINT ( 'NONE',  ( 3.950837973638668288, 0.000000000000000000, 0.000000000000000000 ) ) ;
#10248 = ADVANCED_FACE ( 'NONE', ( #18200, #3180 ), #1771, .F. ) ;
#10249 = SURFACE_STYLE_FILL_AREA ( #2776 ) ;
#10250 = DIRECTION ( 'NONE',  ( -1.000000000000000000, -0.000000000000000000, -0.000000000000000000 ) ) ;
#10251 = CARTESIAN_POINT ( 'NONE',  ( 1.342453679581834924, 14.76648944001039254, -0.9602753779831244563 ) ) ;
#10252 = VECTOR ( 'NONE', #15456, 1000.000000000000114 ) ;
#10253 = DIRECTION ( 'NONE',  ( 0.000000000000000000, 0.000000000000000000, 1.000000000000000000 ) ) ;
#10254 = DIRECTION ( 'NONE',  ( -0.000000000000000000, -0.000000000000000000, 1.000000000000000000 ) ) ;
#10255 = CARTESIAN_POINT ( 'NONE',  ( 0.4862570985993235340, 7.559321496869426227, 11.67702470553367711 ) ) ;
#10256 = VECTOR ( 'NONE', #13482, 1000.000000000000227 ) ;
#10257 = VERTEX_POINT ( 'NONE', #4733 ) ;
#10258 = CARTESIAN_POINT ( 'NONE',  ( 2.002547531651519996, 4.532360870844327039, 11.75462648437103752 ) ) ;
#10259 = CARTESIAN_POINT ( 'NONE',  ( 16.56679352167444819, 0.008252760440870188924, -0.004277682826583317083 ) ) ;
#10260 = VERTEX_POINT ( 'NONE', #10565 ) ;
#10261 = ORIENTED_EDGE ( 'NONE', *, *, #4469, .F. ) ;
#10262 = DIRECTION ( 'NONE',  ( -0.000000000000000000, 1.000000000000000000, -0.000000000000000000 ) ) ;
#10263 = ORIENTED_EDGE ( 'NONE', *, *, #6506, .T. ) ;
#10264 = CARTESIAN_POINT ( 'NONE',  ( 2.636624412714236865, 0.000000000000000000, 0.000000000000000000 ) ) ;
#10265 = EDGE_LOOP ( 'NONE', ( #9779, #4288, #8777, #6487 ) ) ;
#10266 = FACE_OUTER_BOUND ( 'NONE', #7448, .T. ) ;
#10267 = CARTESIAN_POINT ( 'NONE',  ( -66.35602477868049220, 4.999999999999973355, 11.00000000000000000 ) ) ;
#10268 = CARTESIAN_POINT ( 'NONE',  ( 0.3137051932979792457, 4.679953077377485116, 12.91601973349272114 ) ) ;
#10269 = EDGE_CURVE ( 'NONE', #5087, #18124, #4835, .T. ) ;
#10270 = PRODUCT_DEFINITION_SHAPE ( 'NONE', 'NONE',  #12687 ) ;
#10271 = DIRECTION ( 'NONE',  ( 0.000000000000000000, 0.000000000000000000, 1.000000000000000000 ) ) ;
#10272 = CYLINDRICAL_SURFACE ( 'NONE', #3762, 2.500000000000000000 ) ;
#10273 = CARTESIAN_POINT ( 'NONE',  ( 1.861706995891664773, 10.38589138506426934, 6.878962591851789377 ) ) ;
#10274 = CONICAL_SURFACE ( 'NONE', #11808, 14.54644660717763927, 0.8559913436420816257 ) ;
#10275 = CARTESIAN_POINT ( 'NONE',  ( 1.342453679581834924, 5.476372339890016150, 13.74702459364886487 ) ) ;
#10276 = VECTOR ( 'NONE', #12854, 1000.000000000000114 ) ;
#10277 = CARTESIAN_POINT ( 'NONE',  ( 0.3132642857406504611, -7.641821025099783782, -11.41580579227785464 ) ) ;
#10278 = VECTOR ( 'NONE', #7306, 1000.000000000000000 ) ;
#10279 = ORIENTED_EDGE ( 'NONE', *, *, #14843, .F. ) ;
#10280 = CYLINDRICAL_SURFACE ( 'NONE', #17293, 5.000000000000004441 ) ;
#10281 = ORIENTED_EDGE ( 'NONE', *, *, #4070, .T. ) ;
#10282 = VECTOR ( 'NONE', #14921, 1000.000000000000227 ) ;
#10283 = ORIENTED_EDGE ( 'NONE', *, *, #5395, .F. ) ;
#10284 = VERTEX_POINT ( 'NONE', #12990 ) ;
#10285 = EDGE_LOOP ( 'NONE', ( #8480, #11971, #2924, #6464 ) ) ;
#10286 = CARTESIAN_POINT ( 'NONE',  ( 2.002547531651519996, -3.242439124566566910, -12.17374746633581495 ) ) ;
#10287 = CONICAL_SURFACE ( 'NONE', #15186, 2.055000000000000160, 0.7853981633974482790 ) ;
#10288 = DIRECTION ( 'NONE',  ( -1.000000000000000000, 0.000000000000000000, -0.000000000000000000 ) ) ;
#10289 = CARTESIAN_POINT ( 'NONE',  ( 3.950837973638677170, 12.81214529934985080, -6.888253895133152227 ) ) ;
#10290 = ORIENTED_EDGE ( 'NONE', *, *, #10925, .F. ) ;
#10291 = CARTESIAN_POINT ( 'NONE',  ( 2.636624412716062071, -14.14563173255412742, -7.605649742760987486 ) ) ;
#10292 = VECTOR ( 'NONE', #3742, 1000.000000000000000 ) ;
#10293 = EDGE_CURVE ( 'NONE', #16711, #13920, #807, .T. ) ;
#10294 = EDGE_CURVE ( 'NONE', #13957, #10109, #6887, .T. ) ;
#10295 = LINE ( 'NONE', #12212, #6544 ) ;
#10296 = EDGE_CURVE ( 'NONE', #7722, #6395, #11995, .T. ) ;
#10297 = CARTESIAN_POINT ( 'NONE',  ( 1.918918678667047129, -3.258447776119917094, 12.08296592096907318 ) ) ;
#10298 = CARTESIAN_POINT ( 'NONE',  ( 2.002547531651519996, -0.6781519942170860515, -12.57989064830760206 ) ) ;
#10299 = CARTESIAN_POINT ( 'NONE',  ( 1.861628059977343597, -10.38573835516717381, 6.879051339207257421 ) ) ;
#10300 = LINE ( 'NONE', #13253, #4751 ) ;
#10301 = LINE ( 'NONE', #1798, #15383 ) ;
#10302 = CARTESIAN_POINT ( 'NONE',  ( 0.3939822652208129217, -12.90851734139303453, -4.930560016699199188 ) ) ;
#10303 = B_SPLINE_CURVE_WITH_KNOTS ( 'NONE', 3,
 ( #16043, #8788, #14331, #17578, #5616, #8876 ),
 .UNSPECIFIED., .F., .F.,
 ( 4, 2, 4 ),
 ( 3.522439207679730663E-17, 0.0001825746017570575039, 0.0003651492035140797713 ),
 .UNSPECIFIED. ) ;
#10304 =( BOUNDED_SURFACE ( )  B_SPLINE_SURFACE ( 3, 1, ( 
 ( #16208, #3290 ),
 ( #5977, #3092 ),
 ( #15749, #1220 ),
 ( #1878, #18703 ) ),
 .UNSPECIFIED., .F., .F., .T. ) 
 B_SPLINE_SURFACE_WITH_KNOTS ( ( 4, 4 ),
 ( 2, 2 ),
 ( 0.000000000000000000, 1.000000000000000000 ),
 ( 0.000000000000000000, 1.000000000000000000 ),
 .UNSPECIFIED. ) 
 GEOMETRIC_REPRESENTATION_ITEM ( )  RATIONAL_B_SPLINE_SURFACE ( (
 ( 1.000000000000000000, 1.000000000000000000),
 ( 0.7792777138730158093, 0.9689936506012928330),
 ( 0.7792777138730158093, 0.9689936506012928330),
 ( 1.000000000000000000, 1.000000000000000000) ) ) 
 REPRESENTATION_ITEM ( '' )  SURFACE ( )  );
#10305 = CARTESIAN_POINT ( 'NONE',  ( 1.847372867223024073, 7.228345833872753978, 10.12831093686724238 ) ) ;
#10306 = AXIS2_PLACEMENT_3D ( 'NONE', #2093, #18229, #3413 ) ;
#10307 = VERTEX_POINT ( 'NONE', #4304 ) ;
#10308 = EDGE_CURVE ( 'NONE', #17715, #12131, #15122, .T. ) ;
#10309 = ORIENTED_EDGE ( 'NONE', *, *, #7639, .F. ) ;
#10310 = ORIENTED_EDGE ( 'NONE', *, *, #2510, .F. ) ;
#10311 = ORIENTED_EDGE ( 'NONE', *, *, #3733, .T. ) ;
#10312 = CARTESIAN_POINT ( 'NONE',  ( 16.56782317627811096, -0.008141063682853446129, 0.005492611183758502880 ) ) ;
#10313 = VERTEX_POINT ( 'NONE', #10129 ) ;
#10314 = CARTESIAN_POINT ( 'NONE',  ( 0.8740764193768836288, 9.070946295054209685, -11.05257066464527327 ) ) ;
#10315 = CARTESIAN_POINT ( 'NONE',  ( 0.3170788640506441158, -13.11595226728154984, -4.100430649998100030 ) ) ;
#10316 = CARTESIAN_POINT ( 'NONE',  ( 1.977228804422745512, -10.21522664410476366, -11.52787183731191512 ) ) ;
#10317 = CARTESIAN_POINT ( 'NONE',  ( 0.3170788640506441158, -4.392045232375722641, -13.02120094575832709 ) ) ;
#10318 = ORIENTED_EDGE ( 'NONE', *, *, #12264, .F. ) ;
#10319 = FACE_OUTER_BOUND ( 'NONE', #7480, .T. ) ;
#10320 = CIRCLE ( 'NONE', #2095, 2.749999999999998224 ) ;
#10321 = CARTESIAN_POINT ( 'NONE',  ( 3.353306896162456585, 10.44017738170056298, 9.252610477110303933 ) ) ;
#10322 = CARTESIAN_POINT ( 'NONE',  ( 0.4754618798421171855, 0.7484603771384397142, 13.89949764182683012 ) ) ;
#10323 = CARTESIAN_POINT ( 'NONE',  ( 0.4862570985993235340, 12.97920246947886191, -5.003653737315353567 ) ) ;
#10324 = EDGE_CURVE ( 'NONE', #15826, #18802, #9624, .T. ) ;
#10325 = VECTOR ( 'NONE', #1060, 1000.000000000000114 ) ;
#10326 = CARTESIAN_POINT ( 'NONE',  ( -194.9999999999999716, 4.999999999999973355, 6.000000000000005329 ) ) ;
#10327 = ORIENTED_EDGE ( 'NONE', *, *, #2505, .T. ) ;
#10328 = DIRECTION ( 'NONE',  ( -0.000000000000000000, -0.000000000000000000, 1.000000000000000000 ) ) ;
#10330 = ORIENTED_EDGE ( 'NONE', *, *, #15690, .T. ) ;
#10329 = CARTESIAN_POINT ( 'NONE',  ( 1.846138399168762101, 0.4167076046097279440, -12.43476674860266051 ) ) ;
#10331 = EDGE_CURVE ( 'NONE', #5127, #11242, #5967, .T. ) ;
#10332 = CARTESIAN_POINT ( 'NONE',  ( 0.3095370825347234511, 11.38092634279639803, -7.700448427571746635 ) ) ;
#10333 = ORIENTED_EDGE ( 'NONE', *, *, #7772, .T. ) ;
#10334 = FACE_OUTER_BOUND ( 'NONE', #795, .T. ) ;
#10335 = UNCERTAINTY_MEASURE_WITH_UNIT (LENGTH_MEASURE( 1.000000000000000082E-05 ), #244, 'distance_accuracy_value', 'NONE');
#10336 = B_SPLINE_CURVE_WITH_KNOTS ( 'NONE', 3,
 ( #5634, #17308, #4317, #10043, #17401, #5732, #14347, #10239, #7092, #11584, #14440, #5928, #1251 ),
 .UNSPECIFIED., .F., .F.,
 ( 4, 3, 3, 3, 4 ),
 ( 2.453269466693398698E-18, 0.0002299804304191500187, 0.0004599608082120258223, 0.0006467586077648020170, 0.0008336169836825994828 ),
 .UNSPECIFIED. ) ;
#10337 = CARTESIAN_POINT ( 'NONE',  ( 6.500524771653974021, -7.499999999999484857, -12.09892167832712850 ) ) ;
#10338 = ORIENTED_EDGE ( 'NONE', *, *, #9424, .F. ) ;
#10339 = CARTESIAN_POINT ( 'NONE',  ( 5.000000000000006217, -30.00000000000000000, 6.000000000000000000 ) ) ;
#10340 = SURFACE_STYLE_USAGE ( .BOTH. , #7095 ) ;
#10341 = CARTESIAN_POINT ( 'NONE',  ( 3.512766787570770433, -2.025881399556492823, 14.91422000116819113 ) ) ;
#10342 = MANIFOLD_SOLID_BREP ( 'Chamfer2', #7249 ) ;
#10343 = DIRECTION ( 'NONE',  ( -1.000000000000000000, 0.000000000000000000, 0.000000000000000000 ) ) ;
#10344 = ORIENTED_EDGE ( 'NONE', *, *, #15281, .F. ) ;
#10345 = CARTESIAN_POINT ( 'NONE',  ( 0.000000000000000000, 4.769696007084728073, 1.500000000000000000 ) ) ;
#10346 = CARTESIAN_POINT ( 'NONE',  ( 16.57778382496167424, 0.01306626476309378365, 0.007244066302947740205 ) ) ;
#10347 = EDGE_CURVE ( 'NONE', #15522, #13528, #4215, .T. ) ;
#10348 = CARTESIAN_POINT ( 'NONE',  ( 0.3095370825347224519, -8.444334731364081748, 10.84046130709055689 ) ) ;
#10349 = CARTESIAN_POINT ( 'NONE',  ( 0.000000000000000000, 0.000000000000000000, 8.000000000000000000 ) ) ;
#10350 = ORIENTED_EDGE ( 'NONE', *, *, #7083, .F. ) ;
#10351 = CARTESIAN_POINT ( 'NONE',  ( 1.959283090834842200, 4.509128209890970851, 11.71721539537256618 ) ) ;
#10352 = CARTESIAN_POINT ( 'NONE',  ( 0.3137051932979792457, -7.698472063774386420, -11.37800749014139612 ) ) ;
#10353 = B_SPLINE_CURVE_WITH_KNOTS ( 'NONE', 3,
 ( #2666, #10030, #15864, #8600, #7176, #14425 ),
 .UNSPECIFIED., .F., .F.,
 ( 4, 2, 4 ),
 ( 3.144186300207962859E-18, 0.0002017457492448088553, 0.0004034914984896145664 ),
 .UNSPECIFIED. ) ;
#10354 = ORIENTED_EDGE ( 'NONE', *, *, #1307, .F. ) ;
#10355 = ADVANCED_FACE ( 'NONE', ( #2753, #5816 ), #8601, .F. ) ;
#10356 = VERTEX_POINT ( 'NONE', #16454 ) ;
#10357 = CARTESIAN_POINT ( 'NONE',  ( 2.949999999999999734, 3.061616997868383141E-16, -2.500000000000000000 ) ) ;
#10358 = EDGE_LOOP ( 'NONE', ( #93, #9180, #11675, #16418 ) ) ;
#10359 = CARTESIAN_POINT ( 'NONE',  ( 0.4862570985993235340, 7.559321496869426227, 11.67702470553367711 ) ) ;
#10360 = VECTOR ( 'NONE', #13563, 1000.000000000000000 ) ;
#10361 = AXIS2_PLACEMENT_3D ( 'NONE', #1432, #7272, #13084 ) ;
#10362 = VERTEX_POINT ( 'NONE', #17692 ) ;
#10363 = DIRECTION ( 'NONE',  ( -1.224646799147353207E-16, 1.000000000000000000, 0.000000000000000000 ) ) ;
#10364 = SURFACE_SIDE_STYLE ('',( #10560 ) ) ;
#10365 = CARTESIAN_POINT ( 'NONE',  ( 3.950837973638676281, 1.958075594453990487, -14.41405733518058341 ) ) ;
#10366 = CARTESIAN_POINT ( 'NONE',  ( 0.3148208552358936485, 4.463611911212218786, 12.99355031785207260 ) ) ;
#10367 = CIRCLE ( 'NONE', #1514, 2.500000000000000000 ) ;
#10368 = UNCERTAINTY_MEASURE_WITH_UNIT (LENGTH_MEASURE( 1.000000000000000082E-05 ), #6917, 'distance_accuracy_value', 'NONE');
#10369 = CARTESIAN_POINT ( 'NONE',  ( 2.002547531651519996, 9.778737580845815458, -7.942910686618064986 ) ) ;
#10370 = CARTESIAN_POINT ( 'NONE',  ( 16.56679352167444819, 0.001518074900131727951, 0.009170718284672568082 ) ) ;
#10371 = CARTESIAN_POINT ( 'NONE',  ( 1.847426409206469611, 0.06227732482722434654, 12.44303504652092762 ) ) ;
#10372 = CARTESIAN_POINT ( 'NONE',  ( 2.002547531651520885, 10.57595306287292480, 6.845637710436228929 ) ) ;
#10373 = CARTESIAN_POINT ( 'NONE',  ( 2.750000000000000000, 0.000000000000000000, 0.000000000000000000 ) ) ;
#10374 = CARTESIAN_POINT ( 'NONE',  ( -115.3081918537614428, -82.42962774651277869, -87.02631842438563581 ) ) ;
#10375 = EDGE_CURVE ( 'NONE', #1375, #5025, #14878, .T. ) ;
#10376 = CARTESIAN_POINT ( 'NONE',  ( 8.438534575730034959, 1.899950616255187352, 6.598402093327886853 ) ) ;
#10377 = FACE_OUTER_BOUND ( 'NONE', #594, .T. ) ;
#10378 = ORIENTED_EDGE ( 'NONE', *, *, #4634, .T. ) ;
#10379 = EDGE_CURVE ( 'NONE', #4341, #16993, #6214, .T. ) ;
#10380 = VERTEX_POINT ( 'NONE', #8795 ) ;
#10381 = ORIENTED_EDGE ( 'NONE', *, *, #695, .F. ) ;
#10382 = ORIENTED_EDGE ( 'NONE', *, *, #9599, .F. ) ;
#10383 = CARTESIAN_POINT ( 'NONE',  ( 0.3151928479966097374, 6.943324946344315912E-05, 13.73922861026898623 ) ) ;
#10384 = CARTESIAN_POINT ( 'NONE',  ( -194.9999999999999716, 4.999999999999973355, 11.00000000000000000 ) ) ;
#10385 = CARTESIAN_POINT ( 'NONE',  ( 1.560000000000000053, 1.732050807568878747, 7.017607234860990640E-28 ) ) ;
#10386 = ORIENTED_EDGE ( 'NONE', *, *, #15735, .F. ) ;
#10387 = CARTESIAN_POINT ( 'NONE',  ( 0.4862570985993252548, 10.79774104611373353, 8.769551628660776643 ) ) ;
#10388 = DIRECTION ( 'NONE',  ( 0.000000000000000000, 0.000000000000000000, 1.000000000000000000 ) ) ;
#10389 = DIRECTION ( 'NONE',  ( -0.7635533937278214944, 0.6204116510013479857, 0.1790966170213943998 ) ) ;
#10390 = CARTESIAN_POINT ( 'NONE',  ( 16.56822296793089322, -0.003834730849370904075, 0.009385634690641608477 ) ) ;
#10391 = DIRECTION ( 'NONE',  ( 1.000000000000000000, 0.000000000000000000, 0.000000000000000000 ) ) ;
#10392 = B_SPLINE_CURVE_WITH_KNOTS ( 'NONE', 3,
 ( #2795, #11610, #14661, #17442, #11703, #1574, #1484, #4258, #141, #242, #13136, #8641, #7513 ),
 .UNSPECIFIED., .F., .F.,
 ( 4, 3, 3, 3, 4 ),
 ( 3.878959614448864246E-18, 0.0002299780670421047908, 0.0004599561239687891445, 0.0006896788984287886056, 0.0009194956271626397379 ),
 .UNSPECIFIED. ) ;
#10393 = FACE_OUTER_BOUND ( 'NONE', #16245, .T. ) ;
#10394 = CARTESIAN_POINT ( 'NONE',  ( 1.959212340397943120, -9.750290364083578964, -7.909199412631276793 ) ) ;
#10395 = FACE_BOUND ( 'NONE', #6131, .T. ) ;
#10396 = CARTESIAN_POINT ( 'NONE',  ( 1.847168016377982003, 7.464000291196414061, 9.955470380986653822 ) ) ;
#10397 = ORIENTED_EDGE ( 'NONE', *, *, #5158, .T. ) ;
#10398 = ORIENTED_EDGE ( 'NONE', *, *, #4312, .T. ) ;
#10399 = EDGE_CURVE ( 'NONE', #6039, #14233, #18069, .T. ) ;
#10400 = EDGE_LOOP ( 'NONE', ( #10279, #18185, #4992, #3260 ) ) ;
#10401 = VERTEX_POINT ( 'NONE', #1531 ) ;
#10402 = CARTESIAN_POINT ( 'NONE',  ( 16.56782317627811096, 0.007739510688078436902, -0.006045301465876656150 ) ) ;
#10403 = VERTEX_POINT ( 'NONE', #4593 ) ;
#10404 = CARTESIAN_POINT ( 'NONE',  ( 0.3095370825347234511, -11.38092634279634119, 7.700448427571834564 ) ) ;
#10405 = CIRCLE ( 'NONE', #11035, 4.750000000000000000 ) ;
#10406 = CARTESIAN_POINT ( 'NONE',  ( 1.977436885026044200, -13.27782258181834685, 7.806953934146225293 ) ) ;
#10407 = CARTESIAN_POINT ( 'NONE',  ( 2.002547531651521773, 9.778737580845699995, 7.942910686618207983 ) ) ;
#10408 = CARTESIAN_POINT ( 'NONE',  ( 2.636624412714236865, 0.000000000000000000, 0.000000000000000000 ) ) ;
#10409 = ORIENTED_EDGE ( 'NONE', *, *, #11899, .T. ) ;
#10410 = CARTESIAN_POINT ( 'NONE',  ( -3.647233657245695149, 7.499999999999998224, -16.29053473562044019 ) ) ;
#10411 = CARTESIAN_POINT ( 'NONE',  ( -5.000000000000000000, 6.123233995736766282E-16, -6.000000000000000000 ) ) ;
#10412 = CARTESIAN_POINT ( 'NONE',  ( -6.538348415311011408, 7.500000000000000000, -12.00000000000000000 ) ) ;
#10413 = CARTESIAN_POINT ( 'NONE',  ( 0.3720661004400040439, 12.89739157014199833, -4.951033743989506242 ) ) ;
#10414 = ORIENTED_EDGE ( 'NONE', *, *, #15649, .F. ) ;
#10415 =( BOUNDED_SURFACE ( )  B_SPLINE_SURFACE ( 3, 1, ( 
 ( #6824, #2500 ),
 ( #12644, #9692 ),
 ( #9857, #3956 ),
 ( #15694, #15795 ) ),
 .UNSPECIFIED., .F., .F., .T. ) 
 B_SPLINE_SURFACE_WITH_KNOTS ( ( 4, 4 ),
 ( 2, 2 ),
 ( 0.000000000000000000, 1.000000000000000000 ),
 ( 0.000000000000000000, 1.000000000000000000 ),
 .UNSPECIFIED. ) 
 GEOMETRIC_REPRESENTATION_ITEM ( )  RATIONAL_B_SPLINE_SURFACE ( (
 ( 1.000000000000000000, 1.000000000000000000),
 ( 0.9933953342250436691, 0.8357391271907733676),
 ( 0.9933953342250436691, 0.8357391271907733676),
 ( 1.000000000000000000, 1.000000000000000000) ) ) 
 REPRESENTATION_ITEM ( '' )  SURFACE ( )  );
#10416 = CARTESIAN_POINT ( 'NONE',  ( 16.58200780006414732, 0.006043560077721704844, 0.009393638146079782980 ) ) ;
#10417 = CARTESIAN_POINT ( 'NONE',  ( 1.861706995891665439, -6.878962591851823127, 10.38589138506424092 ) ) ;
#10418 = CARTESIAN_POINT ( 'NONE',  ( 16.56679352167444819, 0.004162264567719650525, 0.008311568981097349276 ) ) ;
#10419 = VERTEX_POINT ( 'NONE', #4783 ) ;
#10420 = AXIS2_PLACEMENT_3D ( 'NONE', #4990, #6241, #13496 ) ;
#10421 = DIRECTION ( 'NONE',  ( 0.000000000000000000, 0.000000000000000000, -1.000000000000000000 ) ) ;
#10423 = ORIENTED_EDGE ( 'NONE', *, *, #13199, .T. ) ;
#10422 = CARTESIAN_POINT ( 'NONE',  ( 8.438534575730034959, -6.454982381540271597, -2.341351102130346362 ) ) ;
#10424 = EDGE_CURVE ( 'NONE', #12162, #17649, #10223, .T. ) ;
#10425 = CARTESIAN_POINT ( 'NONE',  ( 0.3137051932979757485, 7.698472063774634222, -11.37800749014122736 ) ) ;
#10426 = EDGE_CURVE ( 'NONE', #5784, #12474, #10793, .T. ) ;
#10427 = EDGE_CURVE ( 'NONE', #8092, #12877, #17785, .T. ) ;
#10428 = FACE_OUTER_BOUND ( 'NONE', #12159, .T. ) ;
#10429 = ORIENTED_EDGE ( 'NONE', *, *, #9195, .F. ) ;
#10430 = DIRECTION ( 'NONE',  ( 0.000000000000000000, 0.000000000000000000, -1.000000000000000000 ) ) ;
#10431 = PRODUCT_DEFINITION_SHAPE ( 'NONE', 'NONE',  #18918 ) ;
#10432 = CARTESIAN_POINT ( 'NONE',  ( 4.545271119321602882, -5.336083332030053583, -11.99999999554311536 ) ) ;
#10433 = ORIENTED_EDGE ( 'NONE', *, *, #16193, .T. ) ;
#10434 = CARTESIAN_POINT ( 'NONE',  ( 1.846822687350018644, 4.121816957446363894, -11.74004266906800353 ) ) ;
#10435 = CARTESIAN_POINT ( 'NONE',  ( 3.950837973638677170, 13.10350451991849141, -6.316429227969337923 ) ) ;
#10436 = DIRECTION ( 'NONE',  ( 0.000000000000000000, 0.000000000000000000, 1.000000000000000000 ) ) ;
#10437 = MANIFOLD_SOLID_BREP ( 'Bore', #834 ) ;
#10438 = VERTEX_POINT ( 'NONE', #12046 ) ;
#10439 = AXIS2_PLACEMENT_3D ( 'NONE', #8318, #953, #2653 ) ;
#10440 = FILL_AREA_STYLE ('',( #17417 ) ) ;
#10441 = LINE ( 'NONE', #16277, #17187 ) ;
#10442 = DIRECTION ( 'NONE',  ( 0.000000000000000000, 0.000000000000000000, 1.000000000000000000 ) ) ;
#10443 = CARTESIAN_POINT ( 'NONE',  ( 16.56822296793089322, 0.005339139727952925060, 0.008619100080558696197 ) ) ;
#10444 = CARTESIAN_POINT ( 'NONE',  ( 0.3307726912345234083, 11.46720933246398388, 7.596084275798933305 ) ) ;
#10445 = DIRECTION ( 'NONE',  ( -1.000000000000000000, 0.000000000000000000, 0.000000000000000000 ) ) ;
#10446 =( BOUNDED_SURFACE ( )  B_SPLINE_SURFACE ( 3, 1, ( 
 ( #6451, #14078 ),
 ( #5281, #15507 ),
 ( #5007, #15322 ),
 ( #6816, #18290 ) ),
 .UNSPECIFIED., .F., .F., .T. ) 
 B_SPLINE_SURFACE_WITH_KNOTS ( ( 4, 4 ),
 ( 2, 2 ),
 ( 0.000000000000000000, 1.000000000000000000 ),
 ( 0.000000000000000000, 1.000000000000000000 ),
 .UNSPECIFIED. ) 
 GEOMETRIC_REPRESENTATION_ITEM ( )  RATIONAL_B_SPLINE_SURFACE ( (
 ( 1.000000000000000000, 1.000000000000000000),
 ( 0.9933953342250436691, 0.8357391271907733676),
 ( 0.9933953342250436691, 0.8357391271907733676),
 ( 1.000000000000000000, 1.000000000000000000) ) ) 
 REPRESENTATION_ITEM ( '' )  SURFACE ( )  );
#10447 = ORIENTED_EDGE ( 'NONE', *, *, #6767, .T. ) ;
#10448 = DIRECTION ( 'NONE',  ( -1.000000000000000000, -0.000000000000000000, -0.000000000000000000 ) ) ;
#10449 = CARTESIAN_POINT ( 'NONE',  ( 0.3095370825347224519, 3.806662003783413351, 13.20347358821915940 ) ) ;
#10450 = ORIENTED_EDGE ( 'NONE', *, *, #13789, .F. ) ;
#10451 = EDGE_CURVE ( 'NONE', #15061, #620, #16352, .T. ) ;
#10452 = ORIENTED_EDGE ( 'NONE', *, *, #9877, .T. ) ;
#10453 = PLANE ( 'NONE',  #261 ) ;
#10454 = EDGE_CURVE ( 'NONE', #14846, #7133, #11089, .T. ) ;
#10455 = VERTEX_POINT ( 'NONE', #3809 ) ;
#10456 = CARTESIAN_POINT ( 'NONE',  ( 0.000000000000000000, 0.000000000000000000, 3.000000000000000000 ) ) ;
#10457 = CIRCLE ( 'NONE', #5936, 16.06066017081991149 ) ;
#10458 = EDGE_LOOP ( 'NONE', ( #9539, #13142 ) ) ;
#10459 = CARTESIAN_POINT ( 'NONE',  ( 1.846138399168762101, 10.30487220521580305, -6.971848976710897539 ) ) ;
#10460 = CARTESIAN_POINT ( 'NONE',  ( 0.3148208552358917056, -13.73693263646118901, 0.2299193288886990094 ) ) ;
#10461 = CARTESIAN_POINT ( 'NONE',  ( 0.3095370825347224519, 0.4597470195090193057, 13.73357284481724960 ) ) ;
#10462 = CARTESIAN_POINT ( 'NONE',  ( -11.50000000000000178, 1.438959988998140357E-15, 11.00000000000000000 ) ) ;
#10463 = B_SPLINE_CURVE_WITH_KNOTS ( 'NONE', 3,
 ( #10703, #16538, #13665, #14278 ),
 .UNSPECIFIED., .F., .F.,
 ( 4, 4 ),
 ( 0.000000000000000000, 0.002004993803842703825 ),
 .UNSPECIFIED. ) ;
#10464 = CIRCLE ( 'NONE', #2221, 16.06066017081991149 ) ;
#10465 = LINE ( 'NONE', #14755, #163 ) ;
#10466 = CARTESIAN_POINT ( 'NONE',  ( 0.3720661004400040439, -7.524064345033547596, 11.58636699658212699 ) ) ;
#10467 = DIRECTION ( 'NONE',  ( -1.000000000000000000, -0.000000000000000000, -0.000000000000000000 ) ) ;
#10468 = DIRECTION ( 'NONE',  ( 0.000000000000000000, 0.000000000000000000, -1.000000000000000000 ) ) ;
#10469 = DIRECTION ( 'NONE',  ( 1.000000000000000000, 0.000000000000000000, 0.000000000000000000 ) ) ;
#10470 = CARTESIAN_POINT ( 'NONE',  ( 3.950837973638675393, -10.05648675950118509, -10.51028938476228980 ) ) ;
#10471 = DIRECTION ( 'NONE',  ( -0.7561779333270775005, 0.6106991889125087392, -0.2350349629540122165 ) ) ;
#10472 = CARTESIAN_POINT ( 'NONE',  ( 0.4754618798421162973, -0.7484603771385398563, 13.89949764182682301 ) ) ;
#10473 = EDGE_CURVE ( 'NONE', #3538, #10284, #5595, .T. ) ;
#10474 = ORIENTED_EDGE ( 'NONE', *, *, #2695, .F. ) ;
#10475 = AXIS2_PLACEMENT_3D ( 'NONE', #1195, #1096, #2519 ) ;
#10476 = ORIENTED_EDGE ( 'NONE', *, *, #15428, .F. ) ;
#10477 = ADVANCED_FACE ( 'NONE', ( #18252 ), #10711, .T. ) ;
#10478 = EDGE_LOOP ( 'NONE', ( #17543, #4173, #2488, #9643 ) ) ;
#10479 = ORIENTED_EDGE ( 'NONE', *, *, #4799, .F. ) ;
#10480 = LINE ( 'NONE', #3198, #6876 ) ;
#10481 = CARTESIAN_POINT ( 'NONE',  ( 1.959212340397961327, 0.6675998551413537818, -12.53706137681889388 ) ) ;
#10482 = ORIENTED_EDGE ( 'NONE', *, *, #15527, .F. ) ;
#10483 = CARTESIAN_POINT ( 'NONE',  ( 0.3939822652208105902, 13.80035637018652395, 0.7002900021918435636 ) ) ;
#10484 = CARTESIAN_POINT ( 'NONE',  ( 2.636624412717099908, 11.60464335004051861, -11.10302021258208249 ) ) ;
#10485 = VERTEX_POINT ( 'NONE', #15201 ) ;
#10486 = CARTESIAN_POINT ( 'NONE',  ( 8.438534575730034959, 6.598402093327880635, 1.899950616255211111 ) ) ;
#10487 = CARTESIAN_POINT ( 'NONE',  ( -997.5739745962155212, 0.000000000000000000, 0.000000000000000000 ) ) ;
#10488 = FACE_OUTER_BOUND ( 'NONE', #11054, .T. ) ;
#10489 = CIRCLE ( 'NONE', #12919, 4.750000000000000000 ) ;
#10490 = EDGE_CURVE ( 'NONE', #13012, #16462, #6545, .T. ) ;
#10491 = AXIS2_PLACEMENT_3D ( 'NONE', #14074, #9234, #5375 ) ;
#10492 = CARTESIAN_POINT ( 'NONE',  ( 1.918918678667044686, -4.466049546133833203, -11.69059232068582865 ) ) ;
#10493 = DIRECTION ( 'NONE',  ( -1.000000000000000000, -0.000000000000000000, -0.000000000000000000 ) ) ;
#10494 = CARTESIAN_POINT ( 'NONE',  ( -26.50000000000001066, -12.50000000000000178, 6.500000000000000888 ) ) ;
#10495 = DIRECTION ( 'NONE',  ( 0.000000000000000000, 0.000000000000000000, 1.000000000000000000 ) ) ;
#10496 = CARTESIAN_POINT ( 'NONE',  ( 1.846138399168762101, 0.4167076046097279440, -12.43476674860266051 ) ) ;
#10497 = ORIENTED_EDGE ( 'NONE', *, *, #8882, .F. ) ;
#10498 = EDGE_LOOP ( 'NONE', ( #6656, #15337, #9998, #1604 ) ) ;
#10499 = ORIENTED_EDGE ( 'NONE', *, *, #10715, .T. ) ;
#10500 = MANIFOLD_SOLID_BREP ( 'AdvancedHole1', #8171 ) ;
#10501 = ORIENTED_EDGE ( 'NONE', *, *, #9265, .T. ) ;
#10502 = CARTESIAN_POINT ( 'NONE',  ( 1.846138399168762101, -7.646096044339819819, -9.815003036200495856 ) ) ;
#10503 = CARTESIAN_POINT ( 'NONE',  ( -205.0000000000000000, -5.000000000000024869, 3.000000000000002665 ) ) ;
#10504 = CONICAL_SURFACE ( 'NONE', #16912, 14.54644660717763927, 0.8559913436420816257 ) ;
#10505 = AXIS2_PLACEMENT_3D ( 'NONE', #17762, #17857, #3013 ) ;
#10506 = CYLINDRICAL_SURFACE ( 'NONE', #2289, 5.000000000000000000 ) ;
#10507 = DIRECTION ( 'NONE',  ( 0.000000000000000000, -0.000000000000000000, -1.000000000000000000 ) ) ;
#10508 = PRODUCT_DEFINITION_FORMATION_WITH_SPECIFIED_SOURCE ( 'ANY', '', #3248, .NOT_KNOWN. ) ;
#10509 = CARTESIAN_POINT ( 'NONE',  ( 0.4862570985993252548, 3.580942890621670482, 13.44146924561382583 ) ) ;
#10510 = ORIENTED_EDGE ( 'NONE', *, *, #2679, .T. ) ;
#10512 = EDGE_CURVE ( 'NONE', #7527, #14389, #8076, .T. ) ;
#10511 = CARTESIAN_POINT ( 'NONE',  ( 1.333872087798561257, 7.499999999999997335, -14.76174338479137838 ) ) ;
#10513 = CARTESIAN_POINT ( 'NONE',  ( 8.438534575730034959, -2.341351102130233119, -6.454982381540311565 ) ) ;
#10514 = CARTESIAN_POINT ( 'NONE',  ( -25.00000000000000000, -2.500000000000000444, -17.00000000000000000 ) ) ;
#10515 = CARTESIAN_POINT ( 'NONE',  ( 1.861628059977342708, 11.66985327793199190, 4.358833901513087916 ) ) ;
#10516 = B_SPLINE_CURVE_WITH_KNOTS ( 'NONE', 3,
 ( #9008, #16082, #3160, #8904 ),
 .UNSPECIFIED., .F., .F.,
 ( 4, 4 ),
 ( 3.727890075251872641E-16, 0.002004993803842877297 ),
 .UNSPECIFIED. ) ;
#10517 = CARTESIAN_POINT ( 'NONE',  ( 16.57210152137263393, -0.003862718596009370557, 0.01402404281923043221 ) ) ;
#10518 = EDGE_CURVE ( 'NONE', #11623, #9992, #9845, .T. ) ;
#10519 = CARTESIAN_POINT ( 'NONE',  ( 2.705023505549863039, 3.294610156756076602, -12.88681800078729189 ) ) ;
#10520 = CARTESIAN_POINT ( 'NONE',  ( 1.959283090834840202, 7.909254450749005017, 9.750336807931171634 ) ) ;
#10521 = ORIENTED_EDGE ( 'NONE', *, *, #12297, .T. ) ;
#10522 = CARTESIAN_POINT ( 'NONE',  ( 2.002547531651519996, -7.942910686618100513, -9.778737580845787036 ) ) ;
#10524 = ORIENTED_EDGE ( 'NONE', *, *, #15998, .T. ) ;
#10523 = CARTESIAN_POINT ( 'NONE',  ( 3.377929128793399016, 10.50432311212916225, -9.234024516648208447 ) ) ;
#10525 = CARTESIAN_POINT ( 'NONE',  ( 0.3939875929385671105, 11.57636969881034084, 7.545068896001249747 ) ) ;
#10526 = CARTESIAN_POINT ( 'NONE',  ( 0.3720661004400040439, 13.79610186261029980, -0.7231997263365288475 ) ) ;
#10527 = VERTEX_POINT ( 'NONE', #8038 ) ;
#10528 = CARTESIAN_POINT ( 'NONE',  ( 0.3308579732647026761, -12.88563776947742312, -4.812490080619330257 ) ) ;
#10529 = CARTESIAN_POINT ( 'NONE',  ( 4.227723179940988452, -5.599337756632702501, -12.00000000790605093 ) ) ;
#10530 =( BOUNDED_SURFACE ( )  B_SPLINE_SURFACE ( 3, 1, ( 
 ( #12957, #5880 ),
 ( #1401, #18789 ),
 ( #5686, #18883 ),
 ( #5783, #11628 ) ),
 .UNSPECIFIED., .F., .F., .T. ) 
 B_SPLINE_SURFACE_WITH_KNOTS ( ( 4, 4 ),
 ( 2, 2 ),
 ( 0.000000000000000000, 1.000000000000000000 ),
 ( 0.000000000000000000, 1.000000000000000000 ),
 .UNSPECIFIED. ) 
 GEOMETRIC_REPRESENTATION_ITEM ( )  RATIONAL_B_SPLINE_SURFACE ( (
 ( 1.000000000000000000, 1.000000000000000000),
 ( 0.9933953342250436691, 0.8357391271907733676),
 ( 0.9933953342250436691, 0.8357391271907733676),
 ( 1.000000000000000000, 1.000000000000000000) ) ) 
 REPRESENTATION_ITEM ( '' )  SURFACE ( )  );
#10531 = ORIENTED_EDGE ( 'NONE', *, *, #11357, .F. ) ;
#10532 = CARTESIAN_POINT ( 'NONE',  ( 1.847412631396506022, 3.886120457021560171, -11.82061107079959861 ) ) ;
#10533 = AXIS2_PLACEMENT_3D ( 'NONE', #94, #1329, #5908 ) ;
#10534 = CARTESIAN_POINT ( 'NONE',  ( 0.3145734862173251711, 13.73540602248380971, 0.3064017202075832724 ) ) ;
#10535 = FACE_OUTER_BOUND ( 'NONE', #9652, .T. ) ;
#10536 = TOROIDAL_SURFACE ( 'NONE', #11442, 3.499999999999992450, 0.5000000000000000000 ) ;
#10537 = CARTESIAN_POINT ( 'NONE',  ( 0.4754618798421171855, 12.98792082933651493, -5.007009103465112076 ) ) ;
#10538 = AXIS2_PLACEMENT_3D ( 'NONE', #11222, #5373, #17038 ) ;
#10539 = EDGE_CURVE ( 'NONE', #13630, #15469, #1339, .T. ) ;
#10540 = EDGE_CURVE ( 'NONE', #2120, #5801, #8057, .T. ) ;
#10541 = EDGE_CURVE ( 'NONE', #15645, #11211, #8476, .T. ) ;
#10542 = VERTEX_POINT ( 'NONE', #14037 ) ;
#10543 = CARTESIAN_POINT ( 'NONE',  ( 1.846138399168762101, -9.815003036200465658, 7.646096044339859787 ) ) ;
#10544 = CARTESIAN_POINT ( 'NONE',  ( 2.002547531651520885, -4.532360870844412304, 11.75462648437100377 ) ) ;
#10545 = CARTESIAN_POINT ( 'NONE',  ( 0.3095370825347233956, 0.4597470195090213041, 13.73357284481724960 ) ) ;
#10546 = CARTESIAN_POINT ( 'NONE',  ( 16.56872352241294521, 0.007512283835804314455, -0.007240717549633915451 ) ) ;
#10547 = CARTESIAN_POINT ( 'NONE',  ( 1.846138399168762101, -0.4167076046094680408, -12.43476674860266940 ) ) ;
#10548 = VECTOR ( 'NONE', #10753, 1000.000000000000000 ) ;
#10549 = ORIENTED_EDGE ( 'NONE', *, *, #2442, .T. ) ;
#10550 = CARTESIAN_POINT ( 'NONE',  ( 0.3148208552358926493, -7.888357771040781508, 11.24855514421872726 ) ) ;
#10551 = CARTESIAN_POINT ( 'NONE',  ( 2.636624412716062960, 6.973567714909310489, -14.46769361191320868 ) ) ;
#10552 = ADVANCED_FACE ( 'NONE', ( #12150 ), #5273, .F. ) ;
#10553 = ORIENTED_EDGE ( 'NONE', *, *, #548, .T. ) ;
#10554 = VERTEX_POINT ( 'NONE', #14120 ) ;
#10555 = CARTESIAN_POINT ( 'NONE',  ( 0.000000000000000000, 0.000000000000000000, -6.000000000000000000 ) ) ;
#10556 = ORIENTED_EDGE ( 'NONE', *, *, #11389, .T. ) ;
#10557 = CARTESIAN_POINT ( 'NONE',  ( 16.58200780006414732, -0.0006320991582348829945, 0.01115192838421569070 ) ) ;
#10558 = VERTEX_POINT ( 'NONE', #12870 ) ;
#10559 =( NAMED_UNIT ( * ) SI_UNIT ( $, .STERADIAN. ) SOLID_ANGLE_UNIT ( ) );
#10560 = SURFACE_STYLE_FILL_AREA ( #4729 ) ;
#10561 = DIRECTION ( 'NONE',  ( 2.891205793294679312E-16, 1.000000000000000000, -0.000000000000000000 ) ) ;
#10562 = CARTESIAN_POINT ( 'NONE',  ( 0.4862570985993235340, -8.769551628660812170, 10.79774104611370333 ) ) ;
#10563 = VECTOR ( 'NONE', #1966, 1000.000000000000227 ) ;
#10564 = CARTESIAN_POINT ( 'NONE',  ( 3.950837973638676281, -14.41405733518061716, 1.958075594453740687 ) ) ;
#10565 = CARTESIAN_POINT ( 'NONE',  ( 3.950837973638676281, -6.316429227969383220, -13.10350451991847009 ) ) ;
#10566 = COLOUR_RGB ( '', 0.09019608, 0.27058824, 0.51372549) ;
#10567 = DIRECTION ( 'NONE',  ( -1.000000000000000000, -0.000000000000000000, -0.000000000000000000 ) ) ;
#10568 = ADVANCED_FACE ( 'NONE', ( #5509 ), #4669, .T. ) ;
#10569 = CARTESIAN_POINT ( 'NONE',  ( -20.00000000000000000, 2.499999999999998668, -16.99999999999999645 ) ) ;
#10570 = EDGE_CURVE ( 'NONE', #10770, #3191, #7148, .T. ) ;
#10571 = DIRECTION ( 'NONE',  ( 0.000000000000000000, 0.000000000000000000, -1.000000000000000000 ) ) ;
#10572 = CARTESIAN_POINT ( 'NONE',  ( 0.3151930723728450512, 13.73922999529477451, 0.07645105376991474799 ) ) ;
#10573 = CARTESIAN_POINT ( 'NONE',  ( 1.846138399168762101, -11.95493567637848109, -3.446241763653124401 ) ) ;
#10574 = CARTESIAN_POINT ( 'NONE',  ( 0.3058872367615226295, 11.46514199369368825, -7.578326039752480092 ) ) ;
#10575 = ORIENTED_EDGE ( 'NONE', *, *, #15649, .T. ) ;
#10576 = ADVANCED_FACE ( 'NONE', ( #3995, #8393 ), #5335, .T. ) ;
#10577 = ORIENTED_EDGE ( 'NONE', *, *, #18476, .T. ) ;
#10578 = ORIENTED_EDGE ( 'NONE', *, *, #10570, .F. ) ;
#10579 = VECTOR ( 'NONE', #14583, 1000.000000000000000 ) ;
#10580 = ORIENTED_EDGE ( 'NONE', *, *, #1398, .T. ) ;
#10581 = MECHANICAL_DESIGN_GEOMETRIC_PRESENTATION_REPRESENTATION (  '', ( #18214 ), #8739 ) ;
#10582 = CARTESIAN_POINT ( 'NONE',  ( 0.3145734862173198421, -7.825584895511444650, -11.29227530924455003 ) ) ;
#10583 = B_SPLINE_CURVE_WITH_KNOTS ( 'NONE', 3,
 ( #6136, #17800, #4701, #10528, #3247, #9095 ),
 .UNSPECIFIED., .F., .F.,
 ( 4, 2, 4 ),
 ( 4.225718824587268470E-17, 0.0002014099069817298145, 0.0004028198139634173993 ),
 .UNSPECIFIED. ) ;
#10584 = CARTESIAN_POINT ( 'NONE',  ( 0.3137051932979757485, 7.698472063774634222, -11.37800749014122736 ) ) ;
#10585 = CARTESIAN_POINT ( 'NONE',  ( 1.959212340397940899, -3.239239832448945755, -12.12975361829679066 ) ) ;
#10586 = DIRECTION ( 'NONE',  ( -1.000000000000000000, -0.000000000000000000, -0.000000000000000000 ) ) ;
#10587 = CARTESIAN_POINT ( 'NONE',  ( 3.950837973638675393, -6.888253895133384930, 12.81214529934972823 ) ) ;
#10588 = CARTESIAN_POINT ( 'NONE',  ( 12.00000000000000711, -19.99999999999999645, 7.000000000000000000 ) ) ;
#10589 = CARTESIAN_POINT ( 'NONE',  ( 16.57210152137263393, -0.003862718596009370557, 0.01402404281923043221 ) ) ;
#10590 = CARTESIAN_POINT ( 'NONE',  ( 0.3720661004400037664, -8.694226082900666341, 10.73619472937699015 ) ) ;
#10591 = FACE_OUTER_BOUND ( 'NONE', #16848, .T. ) ;
#10592 = CARTESIAN_POINT ( 'NONE',  ( 1.254009781011254265, 9.426200207651111995, 11.25324419414182664 ) ) ;
#10593 = B_SPLINE_CURVE_WITH_KNOTS ( 'NONE', 3,
 ( #18598, #1016, #6857, #1661, #17081, #9899 ),
 .UNSPECIFIED., .F., .F.,
 ( 4, 2, 4 ),
 ( 3.229102830436655475E-17, 0.0001825746017570572058, 0.0003651492035140821565 ),
 .UNSPECIFIED. ) ;
#10594 = ADVANCED_FACE ( 'NONE', ( #1215, #12690 ), #2643, .F. ) ;
#10595 = CARTESIAN_POINT ( 'NONE',  ( 0.000000000000000000, 0.000000000000000000, 0.000000000000000000 ) ) ;
#10596 = EDGE_CURVE ( 'NONE', #8651, #5950, #7058, .T. ) ;
#10597 = AXIS2_PLACEMENT_3D ( 'NONE', #12991, #15866, #11573 ) ;
#10598 =( LENGTH_UNIT ( ) NAMED_UNIT ( * ) SI_UNIT ( .MILLI., .METRE. ) );
#10599 = CARTESIAN_POINT ( 'NONE',  ( 1.847380140988739594, 7.402792205949101145, 10.00162556679653214 ) ) ;
#10600 = CIRCLE ( 'NONE', #17287, 14.54644660717763927 ) ;
#10601 = ORIENTED_EDGE ( 'NONE', *, *, #2923, .F. ) ;
#10602 = ADVANCED_FACE ( 'NONE', ( #4088 ), #18726, .T. ) ;
#10603 = ORIENTED_EDGE ( 'NONE', *, *, #10427, .F. ) ;
#10604 = ORIENTED_EDGE ( 'NONE', *, *, #13107, .T. ) ;
#10605 = CIRCLE ( 'NONE', #2049, 8.767949192431130356 ) ;
#10606 = EDGE_LOOP ( 'NONE', ( #8826, #18831, #7899, #12936 ) ) ;
#10607 = CARTESIAN_POINT ( 'NONE',  ( 5.999999999999998224, 20.00000000000000000, 3.000000000000000000 ) ) ;
#10608 = EDGE_CURVE ( 'NONE', #9678, #4154, #13555, .T. ) ;
#10609 = STYLED_ITEM ( 'NONE', ( #3799 ), #16636 ) ;
#10610 = CARTESIAN_POINT ( 'NONE',  ( 0.3132635586635977853, -11.41586812343484070, -7.641727604904016147 ) ) ;
#10611 = DIRECTION ( 'NONE',  ( 0.000000000000000000, 0.000000000000000000, -1.000000000000000000 ) ) ;
#10612 = CARTESIAN_POINT ( 'NONE',  ( 1.846138399168762101, 4.238866729160568170, -11.69739621335917690 ) ) ;
#10613 = CARTESIAN_POINT ( 'NONE',  ( 1.562796894703937678, 0.000000000000000000, 0.000000000000000000 ) ) ;
#10614 = ORIENTED_EDGE ( 'NONE', *, *, #14024, .F. ) ;
#10615 = CARTESIAN_POINT ( 'NONE',  ( 0.3307726912345230752, 3.680742887039495148, -13.25328329128662119 ) ) ;
#10616 = CARTESIAN_POINT ( 'NONE',  ( 0.3142014840576536350, 12.94260032291128759, 4.608051180496968158 ) ) ;
#10617 = FACE_OUTER_BOUND ( 'NONE', #3546, .T. ) ;
#10618 = CARTESIAN_POINT ( 'NONE',  ( 16.56872352241294521, -0.01033355228142402750, 0.001442253899401767583 ) ) ;
#10619 = LINE ( 'NONE', #14708, #16338 ) ;
#10620 = CARTESIAN_POINT ( 'NONE',  ( 0.3148208552358988666, 13.13564827777588917, 4.026279359288469806 ) ) ;
#10621 = ORIENTED_EDGE ( 'NONE', *, *, #2429, .T. ) ;
#10622 = CARTESIAN_POINT ( 'NONE',  ( 2.636624412715137034, -11.60464335004055947, 11.10302021257951743 ) ) ;
#10624 = VERTEX_POINT ( 'NONE', #12782 ) ;
#10623 = CARTESIAN_POINT ( 'NONE',  ( 0.3095370825347224519, 11.38092634279628790, 7.700448427571914500 ) ) ;
#10625 = DIRECTION ( 'NONE',  ( -1.000000000000000000, -0.000000000000000000, 0.000000000000000000 ) ) ;
#10626 = EDGE_CURVE ( 'NONE', #5819, #10871, #2767, .T. ) ;
#10627 = CARTESIAN_POINT ( 'NONE',  ( 16.56782317627811096, -0.008141063682853442660, -0.005492611183757281634 ) ) ;
#10628 = VECTOR ( 'NONE', #1774, 1000.000000000000000 ) ;
#10629 = EDGE_CURVE ( 'NONE', #16167, #12510, #8711, .T. ) ;
#10630 = VERTEX_POINT ( 'NONE', #17003 ) ;
#10631 = CARTESIAN_POINT ( 'NONE',  ( 2.002547531651519996, -0.6781519942170860515, -12.57989064830760206 ) ) ;
#10632 = B_SPLINE_CURVE_WITH_KNOTS ( 'NONE', 3,
 ( #9767, #8348, #2590, #1918, #11948, #15198, #4969, #13671, #1718, #7755, #17689, #4881, #18064 ),
 .UNSPECIFIED., .F., .F.,
 ( 4, 3, 3, 3, 4 ),
 ( 8.673617379884035472E-19, 0.0002299804304191502627, 0.0004599608082120273944, 0.0006467586077648031012, 0.0008336169836825989407 ),
 .UNSPECIFIED. ) ;
#10633 = CARTESIAN_POINT ( 'NONE',  ( -5.682963807814245705, -7.500000000000001776, -12.81889723681861248 ) ) ;
#10634 = VERTEX_POINT ( 'NONE', #4192 ) ;
#10635 = CARTESIAN_POINT ( 'NONE',  ( 0.3095370825347224519, 13.20347358821919670, -3.806662003783277459 ) ) ;
#10636 = CARTESIAN_POINT ( 'NONE',  ( 2.002547531651519996, 0.6781519942171739812, 12.57989064830759851 ) ) ;
#10637 = CARTESIAN_POINT ( 'NONE',  ( 0.3939822652208094800, -7.545099438011941828, -11.57634296752776137 ) ) ;
#10638 = CARTESIAN_POINT ( 'NONE',  ( 0.3308579732647051186, 3.680601586799872482, 13.25341063505876882 ) ) ;
#10639 = ORIENTED_EDGE ( 'NONE', *, *, #1185, .T. ) ;
#10640 = B_SPLINE_CURVE_WITH_KNOTS ( 'NONE', 3,
 ( #11996, #2064, #4834, #4924, #8240, #18356, #18020 ),
 .UNSPECIFIED., .F., .F.,
 ( 4, 3, 4 ),
 ( 3.198396408832238080E-18, 0.0002299780670421062274, 0.0004597478348664300451 ),
 .UNSPECIFIED. ) ;
#10641 = SHAPE_REPRESENTATION_RELATIONSHIP ( 'NONE' , 'NONE' ,  #6437, #14891 ) ;
#10642 = CARTESIAN_POINT ( 'NONE',  ( 1.845755665166725068, 12.43231320373361193, 0.4784952423728983106 ) ) ;
#10643 = CARTESIAN_POINT ( 'NONE',  ( 1.846138399168762989, -4.238866729160486457, 11.69739621335920710 ) ) ;
#10644 = DIRECTION ( 'NONE',  ( 0.000000000000000000, 0.000000000000000000, 1.000000000000000000 ) ) ;
#10646 = VERTEX_POINT ( 'NONE', #10006 ) ;
#10645 = DIRECTION ( 'NONE',  ( 1.000000000000000000, 0.000000000000000000, 0.000000000000000000 ) ) ;
#10647 = CARTESIAN_POINT ( 'NONE',  ( 0.4862570985993235340, -12.97920246947883172, 5.003653737315437944 ) ) ;
#10648 = VERTEX_POINT ( 'NONE', #1310 ) ;
#10649 = CARTESIAN_POINT ( 'NONE',  ( 0.3148208552358935375, -4.026279359288518656, 13.13564827777588029 ) ) ;
#10650 = CARTESIAN_POINT ( 'NONE',  ( 1.845756295923356438, -11.67600463554276224, 4.296776483139434610 ) ) ;
#10651 =( BOUNDED_SURFACE ( )  B_SPLINE_SURFACE ( 3, 1, ( 
 ( #3046, #4791 ),
 ( #13288, #203 ),
 ( #8989, #17704 ),
 ( #3346, #1630 ) ),
 .UNSPECIFIED., .F., .F., .T. ) 
 B_SPLINE_SURFACE_WITH_KNOTS ( ( 4, 4 ),
 ( 2, 2 ),
 ( 0.000000000000000000, 1.000000000000000000 ),
 ( 0.000000000000000000, 1.000000000000000000 ),
 .UNSPECIFIED. ) 
 GEOMETRIC_REPRESENTATION_ITEM ( )  RATIONAL_B_SPLINE_SURFACE ( (
 ( 1.000000000000000000, 1.000000000000000000),
 ( 0.9593108457356467333, 0.9995965569486454649),
 ( 0.9593108457356467333, 0.9995965569486454649),
 ( 1.000000000000000000, 1.000000000000000000) ) ) 
 REPRESENTATION_ITEM ( '' )  SURFACE ( )  );
#10652 = ORIENTED_EDGE ( 'NONE', *, *, #909, .F. ) ;
#10653 = EDGE_CURVE ( 'NONE', #10095, #8886, #11902, .T. ) ;
#10654 = EDGE_CURVE ( 'NONE', #18897, #5701, #15989, .T. ) ;
#10655 = EDGE_CURVE ( 'NONE', #12889, #2783, #3704, .T. ) ;
#10656 = ORIENTED_EDGE ( 'NONE', *, *, #16880, .F. ) ;
#10657 = LINE ( 'NONE', #12182, #10011 ) ;
#10658 = EDGE_LOOP ( 'NONE', ( #10382, #5946, #6675 ) ) ;
#10659 = CARTESIAN_POINT ( 'NONE',  ( 0.4754618798421167414, 10.80499583390513152, 8.775436892861154803 ) ) ;
#10660 = ORIENTED_EDGE ( 'NONE', *, *, #16862, .T. ) ;
#10661 = PLANE ( 'NONE',  #9176 ) ;
#10662 = DIRECTION ( 'NONE',  ( 0.000000000000000000, 1.000000000000000000, 0.000000000000000000 ) ) ;
#10663 = CARTESIAN_POINT ( 'NONE',  ( 1.254009781012255020, 7.789615163754674221, -12.44229282923133262 ) ) ;
#10664 = LINE ( 'NONE', #3379, #16944 ) ;
#10665 = CARTESIAN_POINT ( 'NONE',  ( -30.00000000000000355, -12.50000000000000178, 7.000000000000000000 ) ) ;
#10666 = CARTESIAN_POINT ( 'NONE',  ( 0.3720661004400037664, -4.951033743989731839, 12.89739157014191129 ) ) ;
#10667 = CARTESIAN_POINT ( 'NONE',  ( 2.002547531651519996, -3.242439124566566910, -12.17374746633581495 ) ) ;
#10668 = CARTESIAN_POINT ( 'NONE',  ( 0.3151930723728398331, 8.013866567350898862, 11.16020735774769435 ) ) ;
#10669 = CARTESIAN_POINT ( 'NONE',  ( 1.254255976357308233, 13.61551404021196277, 5.487601330834896096 ) ) ;
#10670 = CARTESIAN_POINT ( 'NONE',  ( 16.56679352167444819, -0.008252760440870216679, 0.004277682826583264174 ) ) ;
#10671 = FILL_AREA_STYLE_COLOUR ( '', #6618 ) ;
#10672 = VECTOR ( 'NONE', #10246, 1000.000000000000114 ) ;
#10673 = ORIENTED_EDGE ( 'NONE', *, *, #4539, .T. ) ;
#10674 = VECTOR ( 'NONE', #14138, 1000.000000000000000 ) ;
#10675 = EDGE_CURVE ( 'NONE', #4457, #12775, #15543, .T. ) ;
#10676 = EDGE_CURVE ( 'NONE', #2096, #11053, #10301, .T. ) ;
#10677 = EDGE_CURVE ( 'NONE', #18537, #1902, #14635, .T. ) ;
#10678 = ORIENTED_EDGE ( 'NONE', *, *, #10218, .F. ) ;
#10679 = ORIENTED_EDGE ( 'NONE', *, *, #195, .F. ) ;
#10680 = ORIENTED_EDGE ( 'NONE', *, *, #3412, .T. ) ;
#10681 = EDGE_CURVE ( 'NONE', #78, #9622, #6891, .T. ) ;
#10682 = CARTESIAN_POINT ( 'NONE',  ( 0.3150692679896004988, 4.099798979280845579, 13.11337225490253644 ) ) ;
#10683 = CARTESIAN_POINT ( 'NONE',  ( 0.3132642857406529591, -13.72733058964894681, -0.5276792104583708509 ) ) ;
#10684 = PLANE ( 'NONE',  #15744 ) ;
#10685 = CARTESIAN_POINT ( 'NONE',  ( 2.002547531651519996, 0.6781519942171739812, 12.57989064830759851 ) ) ;
#10686 = DIRECTION ( 'NONE',  ( 0.000000000000000000, 0.000000000000000000, 1.000000000000000000 ) ) ;
#10687 = VECTOR ( 'NONE', #13771, 1000.000000000000000 ) ;
#10688 = CARTESIAN_POINT ( 'NONE',  ( 0.4754618798421167414, 7.564402563418470393, 11.68486377711969126 ) ) ;
#10689 = LINE ( 'NONE', #1988, #661 ) ;
#10690 = CARTESIAN_POINT ( 'NONE',  ( 1.254009781011994340, -1.011465182608154434, -14.64464726212624690 ) ) ;
#10691 = CARTESIAN_POINT ( 'NONE',  ( 15.00000000000000711, -45.00000000000000000, 3.000000000000000000 ) ) ;
#10692 = CARTESIAN_POINT ( 'NONE',  ( 22.75000000000000000, 0.000000000000000000, 0.000000000000000000 ) ) ;
#10693 = CARTESIAN_POINT ( 'NONE',  ( 2.636624412714236865, 0.000000000000000000, 0.000000000000000000 ) ) ;
#10694 = DIRECTION ( 'NONE',  ( -0.000000000000000000, -0.000000000000000000, 1.000000000000000000 ) ) ;
#10695 = VERTEX_POINT ( 'NONE', #14592 ) ;
#10696 = ORIENTED_EDGE ( 'NONE', *, *, #1753, .F. ) ;
#10697 = ORIENTED_EDGE ( 'NONE', *, *, #14086, .T. ) ;
#10698 = ORIENTED_EDGE ( 'NONE', *, *, #11591, .T. ) ;
#10699 = CARTESIAN_POINT ( 'NONE',  ( 3.950837973638676281, -6.888253895133199300, -12.81214529934982949 ) ) ;
#10700 = CARTESIAN_POINT ( 'NONE',  ( 0.3720661004400037664, -11.58636699658219982, 7.524064345033424139 ) ) ;
#10701 = EDGE_CURVE ( 'NONE', #6249, #8937, #4143, .T. ) ;
#10702 = LINE ( 'NONE', #16537, #5625 ) ;
#10703 = CARTESIAN_POINT ( 'NONE',  ( 3.950837973638676281, -12.81214529934979929, 6.888253895133251703 ) ) ;
#10704 = CARTESIAN_POINT ( 'NONE',  ( 3.950837973638677170, -14.31366178983255466, 2.591948120961746760 ) ) ;
#10705 = ORIENTED_EDGE ( 'NONE', *, *, #8699, .F. ) ;
#10706 = CARTESIAN_POINT ( 'NONE',  ( 0.3308579732647026761, -0.5950689966505304795, 13.74211098745268522 ) ) ;
#10707 = CARTESIAN_POINT ( 'NONE',  ( 0.4754618798421162973, -7.564402563418381575, -11.68486377711974811 ) ) ;
#10708 = CARTESIAN_POINT ( 'NONE',  ( -5.084818453916207126, 7.500000000000262013, -13.03762002034318357 ) ) ;
#10709 = CARTESIAN_POINT ( 'NONE',  ( 0.3095370825347233956, 12.91933430393614302, -4.681152801286028620 ) ) ;
#10710 = DIRECTION ( 'NONE',  ( 0.000000000000000000, 1.000000000000000000, 0.000000000000000000 ) ) ;
#10711 = CYLINDRICAL_SURFACE ( 'NONE', #2806, 7.000000000000000000 ) ;
#10712 = CARTESIAN_POINT ( 'NONE',  ( 2.636624412714236865, 0.000000000000000000, 0.000000000000000000 ) ) ;
#10713 = VERTEX_POINT ( 'NONE', #13254 ) ;
#10714 = B_SPLINE_CURVE_WITH_KNOTS ( 'NONE', 3,
 ( #12068, #4806, #4411, #10638, #8811, #9193 ),
 .UNSPECIFIED., .F., .F.,
 ( 4, 2, 4 ),
 ( 4.063025038712889623E-17, 0.0002014099069817291640, 0.0004028198139634176704 ),
 .UNSPECIFIED. ) ;
#10715 = EDGE_CURVE ( 'NONE', #14742, #11007, #13357, .T. ) ;
#10716 = FACE_OUTER_BOUND ( 'NONE', #682, .T. ) ;
#10718 = ORIENTED_EDGE ( 'NONE', *, *, #6340, .F. ) ;
#10717 = CARTESIAN_POINT ( 'NONE',  ( 0.4862570985993235340, -8.769551628660655851, -10.79774104611382946 ) ) ;
#10719 = CARTESIAN_POINT ( 'NONE',  ( 0.3132642857406554571, 12.89240536501346313, 4.743831191224429311 ) ) ;
#10720 = CARTESIAN_POINT ( 'NONE',  ( 0.4754618798421162973, 11.68486377711977475, -7.564402563418339831 ) ) ;
#10721 = EDGE_LOOP ( 'NONE', ( #16750, #8091, #2376, #14962, #1418 ) ) ;
#10722 = CARTESIAN_POINT ( 'NONE',  ( 16.56753206892534891, 0.006669401563385194548, 0.006760771273035138390 ) ) ;
#10723 = CARTESIAN_POINT ( 'NONE',  ( -1.070106460717440422, -7.499999999999997335, -13.06798451319506249 ) ) ;
#10724 = ORIENTED_EDGE ( 'NONE', *, *, #10758, .T. ) ;
#10725 = DIRECTION ( 'NONE',  ( -1.000000000000000000, 0.000000000000000000, 0.000000000000000000 ) ) ;
#10726 = CARTESIAN_POINT ( 'NONE',  ( 0.3308579732647007887, -10.76782854710821269, -8.558831104907037357 ) ) ;
#10727 = CARTESIAN_POINT ( 'NONE',  ( 1.846138399168762989, 11.69739621335922308, 4.238866729160444713 ) ) ;
#10728 = FACE_BOUND ( 'NONE', #12265, .T. ) ;
#10729 = CIRCLE ( 'NONE', #17126, 5.000000000000004441 ) ;
#10730 = ORIENTED_EDGE ( 'NONE', *, *, #16141, .T. ) ;
#10731 = ADVANCED_FACE ( 'NONE', ( #1511 ), #16403, .F. ) ;
#10732 = SURFACE_STYLE_USAGE ( .BOTH. , #7970 ) ;
#10733 = CARTESIAN_POINT ( 'NONE',  ( 3.950837973638676281, -14.41405733518059229, -1.958075594453940971 ) ) ;
#10734 = B_SPLINE_CURVE_WITH_KNOTS ( 'NONE', 3,
 ( #6169, #7996, #12001, #5111, #6553, #3673 ),
 .UNSPECIFIED., .F., .F.,
 ( 4, 2, 4 ),
 ( 0.000000000000000000, 0.001656992708823640335, 0.003313985417647279802 ),
 .UNSPECIFIED. ) ;
#10735 = FACE_OUTER_BOUND ( 'NONE', #13191, .T. ) ;
#10737 = ORIENTED_EDGE ( 'NONE', *, *, #12462, .T. ) ;
#10736 = DIRECTION ( 'NONE',  ( 1.000000000000000000, 0.000000000000000000, -0.000000000000000000 ) ) ;
#10738 = CARTESIAN_POINT ( 'NONE',  ( 16.56822296793089322, -0.01011126603341077138, 0.0007467251401298242519 ) ) ;
#10739 = EDGE_CURVE ( 'NONE', #4587, #5121, #4471, .T. ) ;
#10740 = ORIENTED_EDGE ( 'NONE', *, *, #3044, .T. ) ;
#10741 = CARTESIAN_POINT ( 'NONE',  ( 2.123976203522053741, -1.531817366691644144, -15.54801196254788742 ) ) ;
#10742 = VERTEX_POINT ( 'NONE', #17670 ) ;
#10743 = EDGE_LOOP ( 'NONE', ( #9302, #8427, #12575, #10521, #4774, #3698 ) ) ;
#10744 = CARTESIAN_POINT ( 'NONE',  ( 0.3145729642390365788, 10.93201268464384768, -8.321438378985135387 ) ) ;
#10745 = ORIENTED_EDGE ( 'NONE', *, *, #8499, .T. ) ;
#10746 = DIRECTION ( 'NONE',  ( 0.000000000000000000, 0.000000000000000000, -1.000000000000000000 ) ) ;
#10747 = ORIENTED_EDGE ( 'NONE', *, *, #10681, .F. ) ;
#10748 = FILL_AREA_STYLE_COLOUR ( '', #5963 ) ;
#10749 =( LENGTH_UNIT ( ) NAMED_UNIT ( * ) SI_UNIT ( .MILLI., .METRE. ) );
#10750 = B_SPLINE_CURVE_WITH_KNOTS ( 'NONE', 3,
 ( #11056, #5124, #2252, #12385, #12475, #12564 ),
 .UNSPECIFIED., .F., .F.,
 ( 4, 2, 4 ),
 ( 3.499941646806256644E-17, 0.0001825746017570586152, 0.0003651492035140799881 ),
 .UNSPECIFIED. ) ;
#10751 = CARTESIAN_POINT ( 'NONE',  ( 1.500000000000000000, 2.869946927167511679E-16, 5.000000000000000000 ) ) ;
#10752 = CIRCLE ( 'NONE', #3414, 2.499999999999995115 ) ;
#10753 = DIRECTION ( 'NONE',  ( -0.000000000000000000, -0.000000000000000000, -1.000000000000000000 ) ) ;
#10754 = DIRECTION ( 'NONE',  ( 0.000000000000000000, 0.000000000000000000, 1.000000000000000000 ) ) ;
#10755 = PRODUCT ( 'Handle Arm 1', 'Handle Arm 1', '', ( #9501 ) ) ;
#10756 = CARTESIAN_POINT ( 'NONE',  ( 1.918918678667046462, 7.860057224348842020, 9.738328798462404734 ) ) ;
#10757 = CARTESIAN_POINT ( 'NONE',  ( 0.000000000000000000, 0.000000000000000000, 0.000000000000000000 ) ) ;
#10758 = EDGE_CURVE ( 'NONE', #1712, #17181, #6457, .T. ) ;
#10759 = FILL_AREA_STYLE ('',( #13517 ) ) ;
#10760 = CARTESIAN_POINT ( 'NONE',  ( 1.918918678667044686, -10.48466773720556766, -6.832809802519125064 ) ) ;
#10761 = EDGE_CURVE ( 'NONE', #11623, #1184, #10464, .T. ) ;
#10762 = CARTESIAN_POINT ( 'NONE',  ( 1.977436885026506497, -3.321781585408274839, -15.04044112860335147 ) ) ;
#10763 = CARTESIAN_POINT ( 'NONE',  ( 0.3137051932979757485, 8.442169467526850823, 10.83767969834806166 ) ) ;
#10764 = CARTESIAN_POINT ( 'NONE',  ( 8.438534575730034959, -4.221456476902624821, -5.415535776177568650 ) ) ;
#10765 = CARTESIAN_POINT ( 'NONE',  ( 1.846138399168762101, -11.69739621335925328, 4.238866729160359448 ) ) ;
#10766 = CIRCLE ( 'NONE', #15620, 5.000000000000000000 ) ;
#10767 = CARTESIAN_POINT ( 'NONE',  ( 16.57210152137263393, -0.005118120558001483002, 0.01361613799508852585 ) ) ;
#10768 = ORIENTED_EDGE ( 'NONE', *, *, #12164, .F. ) ;
#10769 = ORIENTED_EDGE ( 'NONE', *, *, #18131, .F. ) ;
#10770 = VERTEX_POINT ( 'NONE', #9057 ) ;
#10771 = ORIENTED_EDGE ( 'NONE', *, *, #13916, .T. ) ;
#10772 = ORIENTED_EDGE ( 'NONE', *, *, #6124, .T. ) ;
#10773 = CARTESIAN_POINT ( 'NONE',  ( -4.505465888036638944, -19.31487138727242225, 3.000000000000000000 ) ) ;
#10774 = CARTESIAN_POINT ( 'NONE',  ( 2.863953186090933745, -7.500000000000002665, -15.84864299207353433 ) ) ;
#10775 = CARTESIAN_POINT ( 'NONE',  ( -205.0000000000000000, 4.999999999999975131, -153.7432847437423789 ) ) ;
#10776 = PRODUCT_DEFINITION_CONTEXT ( 'detailed design', #5684, 'design' ) ;
#10777 = ORIENTED_EDGE ( 'NONE', *, *, #8942, .T. ) ;
#10778 = CARTESIAN_POINT ( 'NONE',  ( 2.747332970342022840, 7.555624153089646633, 14.49942876448594831 ) ) ;
#10779 = CARTESIAN_POINT ( 'NONE',  ( 2.747332970342022840, 16.17136872824898575, 2.409922051470737348 ) ) ;
#10780 = EDGE_CURVE ( 'NONE', #18854, #17057, #12110, .T. ) ;
#10781 = DIRECTION ( 'NONE',  ( -1.000000000000000000, 0.000000000000000000, 0.000000000000000000 ) ) ;
#10782 = EDGE_CURVE ( 'NONE', #4268, #15230, #12891, .T. ) ;
#10783 = CARTESIAN_POINT ( 'NONE',  ( 0.000000000000000000, 0.000000000000000000, 8.000000000000000000 ) ) ;
#10784 = EDGE_CURVE ( 'NONE', #4406, #16984, #13822, .T. ) ;
#10785 = DIRECTION ( 'NONE',  ( 1.000000000000000000, 0.000000000000000000, 0.000000000000000000 ) ) ;
#10786 = CARTESIAN_POINT ( 'NONE',  ( 1.846138399168762101, 7.646096044340033870, -9.815003036200328879 ) ) ;
#10787 = CIRCLE ( 'NONE', #999, 12.00000000000000178 ) ;
#10788 = EDGE_LOOP ( 'NONE', ( #11592, #1296, #1929, #16733 ) ) ;
#10789 = B_SPLINE_CURVE_WITH_KNOTS ( 'NONE', 3,
 ( #1163, #1061, #2766, #4228 ),
 .UNSPECIFIED., .F., .F.,
 ( 4, 4 ),
 ( 0.000000000000000000, 0.002004993803841771411 ),
 .UNSPECIFIED. ) ;
#10790 = ORIENTED_EDGE ( 'NONE', *, *, #623, .T. ) ;
#10791 = ORIENTED_EDGE ( 'NONE', *, *, #7260, .T. ) ;
#10792 = ORIENTED_EDGE ( 'NONE', *, *, #2909, .F. ) ;
#10793 = B_SPLINE_CURVE_WITH_KNOTS ( 'NONE', 3,
 ( #16252, #7373, #13471, #3134, #293, #14710, #13183, #8980, #1921, #10620, #1722, #99, #6123 ),
 .UNSPECIFIED., .F., .F.,
 ( 4, 3, 3, 3, 4 ),
 ( 1.734723475976807094E-18, 0.0002299780670421060647, 0.0004599561239687893072, 0.0006896788984287890393, 0.0009194956271626404968 ),
 .UNSPECIFIED. ) ;
#10794 = DIRECTION ( 'NONE',  ( 0.000000000000000000, 0.000000000000000000, 1.000000000000000000 ) ) ;
#10795 = CARTESIAN_POINT ( 'NONE',  ( 16.57210152137263393, 0.005118120558001383255, -0.01361613799508856922 ) ) ;
#10796 = CARTESIAN_POINT ( 'NONE',  ( 1.847168016377979116, -7.464000291196340342, -9.955470380986712442 ) ) ;
#10797 = CARTESIAN_POINT ( 'NONE',  ( 3.950837973638676281, -6.316429227969562632, 13.10350451991838128 ) ) ;
#10798 = CARTESIAN_POINT ( 'NONE',  ( 0.4862570985993235340, 7.559321496869593204, -11.67702470553357053 ) ) ;
#10799 = ORIENTED_EDGE ( 'NONE', *, *, #875, .T. ) ;
#10800 = CARTESIAN_POINT ( 'NONE',  ( 1.846138399168762989, -4.238866729160486457, 11.69739621335920710 ) ) ;
#10801 = CONICAL_SURFACE ( 'NONE', #2523, 16.06066017081991149, 0.7853981625000062694 ) ;
#10802 = DIRECTION ( 'NONE',  ( 1.000000000000000000, 0.000000000000000000, 0.000000000000000000 ) ) ;
#10803 = CARTESIAN_POINT ( 'NONE',  ( -6.265543861956235361, 7.499999999999998224, -12.41474642440600640 ) ) ;
#10804 = CARTESIAN_POINT ( 'NONE',  ( 0.4862570985993235340, -10.79774104611379215, 8.769551628660700260 ) ) ;
#10805 = DIRECTION ( 'NONE',  ( 0.000000000000000000, 0.000000000000000000, -1.000000000000000000 ) ) ;
#10806 = CARTESIAN_POINT ( 'NONE',  ( 3.353306896162455697, -1.348936822032921423, 13.88482890973696016 ) ) ;
#10807 = DIRECTION ( 'NONE',  ( -1.000000000000000000, 0.000000000000000000, 0.000000000000000000 ) ) ;
#10808 = ORIENTED_EDGE ( 'NONE', *, *, #8490, .T. ) ;
#10809 = EDGE_CURVE ( 'NONE', #7261, #10646, #15353, .T. ) ;
#10810 = EDGE_CURVE ( 'NONE', #17093, #492, #15078, .T. ) ;
#10811 = ORIENTED_EDGE ( 'NONE', *, *, #143, .F. ) ;
#10812 = CARTESIAN_POINT ( 'NONE',  ( 1.845756295923357104, 11.67600463554279244, -4.296776483139357339 ) ) ;
#10813 = AXIS2_PLACEMENT_3D ( 'NONE', #2910, #13059, #4082 ) ;
#10814 = EDGE_CURVE ( 'NONE', #15883, #9927, #1848, .T. ) ;
#10815 = ORIENTED_EDGE ( 'NONE', *, *, #403, .T. ) ;
#10816 = CARTESIAN_POINT ( 'NONE',  ( 1.847461586945734480, -3.877048136045296634, -11.82388984758122596 ) ) ;
#10817 = CARTESIAN_POINT ( 'NONE',  ( 0.3417098569972104594, -7.500000000000000888, -14.22469181348825096 ) ) ;
#10818 = EDGE_LOOP ( 'NONE', ( #17115, #18858, #7215, #778, #4865, #1393 ) ) ;
#10819 = CARTESIAN_POINT ( 'NONE',  ( -30.00000000000000711, 20.00000000000000000, 0.000000000000000000 ) ) ;
#10820 = CARTESIAN_POINT ( 'NONE',  ( 16.57210152137263393, 0.003862718596009469003, -0.01402404281923040792 ) ) ;
#10821 = DIRECTION ( 'NONE',  ( 1.000000000000000000, 0.000000000000000000, 0.000000000000000000 ) ) ;
#10822 = DIRECTION ( 'NONE',  ( 0.000000000000000000, 0.000000000000000000, 1.000000000000000000 ) ) ;
#10823 = B_SPLINE_CURVE_WITH_KNOTS ( 'NONE', 3,
 ( #10470, #151, #11711, #16204 ),
 .UNSPECIFIED., .F., .F.,
 ( 4, 4 ),
 ( 2.117499858742978245E-17, 0.003005512676784849197 ),
 .UNSPECIFIED. ) ;
#10824 = AXIS2_PLACEMENT_3D ( 'NONE', #6242, #17618, #17513 ) ;
#10825 = PRODUCT_RELATED_PRODUCT_CATEGORY ( 'part', '', ( #537 ) ) ;
#10826 = EDGE_CURVE ( 'NONE', #10770, #1445, #3508, .T. ) ;
#10827 = PRODUCT_DEFINITION_FORMATION_WITH_SPECIFIED_SOURCE ( 'ANY', '', #206, .NOT_KNOWN. ) ;
#10828 = B_SPLINE_CURVE_WITH_KNOTS ( 'NONE', 3,
 ( #12829, #18477, #11232, #8355, #14172, #1078, #2419, #8269, #14084, #18569, #990, #6825, #15425 ),
 .UNSPECIFIED., .F., .F.,
 ( 4, 3, 3, 3, 4 ),
 ( 8.673617379884035472E-19, 0.0002299804304191491514, 0.0004599608082120254429, 0.0006467586077648011496, 0.0008336169836825998080 ),
 .UNSPECIFIED. ) ;
#10829 = CARTESIAN_POINT ( 'NONE',  ( 1.861706995891665439, -6.878962591851823127, 10.38589138506424092 ) ) ;
#10830 = ADVANCED_FACE ( 'NONE', ( #6294 ), #18337, .F. ) ;
#10831 = EDGE_CURVE ( 'NONE', #14846, #16237, #95, .T. ) ;
#10832 = LINE ( 'NONE', #5082, #3402 ) ;
#10834 = ORIENTED_EDGE ( 'NONE', *, *, #9782, .T. ) ;
#10833 = DIRECTION ( 'NONE',  ( -1.000000000000000000, -1.577021341797097560E-16, 0.000000000000000000 ) ) ;
#10835 = DIRECTION ( 'NONE',  ( -0.000000000000000000, 0.5000000000000003331, -0.8660254037844384856 ) ) ;
#10836 = ORIENTED_EDGE ( 'NONE', *, *, #17242, .T. ) ;
#10837 = CARTESIAN_POINT ( 'NONE',  ( 1.861628059977341598, 12.00316790821106139, -3.332996951203504032 ) ) ;
#10838 = CARTESIAN_POINT ( 'NONE',  ( 0.4754618798421162973, -13.45049478164062329, 3.583352865732616355 ) ) ;
#10839 = EDGE_LOOP ( 'NONE', ( #2925, #7760, #18803, #17475, #8071, #16549, #4998, #9947 ) ) ;
#10840 = AXIS2_PLACEMENT_3D ( 'NONE', #15925, #2725, #10191 ) ;
#10841 = ORIENTED_EDGE ( 'NONE', *, *, #6601, .F. ) ;
#10842 = CARTESIAN_POINT ( 'NONE',  ( 1.847247051441591514, -0.1676840720646167182, 12.44188156437794213 ) ) ;
#10843 = VERTEX_POINT ( 'NONE', #15176 ) ;
#10844 = DIRECTION ( 'NONE',  ( -0.000000000000000000, -0.000000000000000000, 1.000000000000000000 ) ) ;
#10845 = ADVANCED_BREP_SHAPE_REPRESENTATION ( '', ( #3589, #2030 ), #1089 ) ;
#10846 = ORIENTED_EDGE ( 'NONE', *, *, #14437, .T. ) ;
#10847 = TOROIDAL_SURFACE ( 'NONE', #15395, 11.50000000000000178, 0.5000000000000000000 ) ;
#10848 = FACE_OUTER_BOUND ( 'NONE', #7221, .T. ) ;
#10849 = EDGE_CURVE ( 'NONE', #13318, #14429, #10787, .T. ) ;
#10850 = CARTESIAN_POINT ( 'NONE',  ( 0.4862570985993252548, 5.003653737315486794, 12.97920246947881395 ) ) ;
#10851 = FILL_AREA_STYLE_COLOUR ( '', #3636 ) ;
#10852 = LINE ( 'NONE', #2233, #13278 ) ;
#10853 = CARTESIAN_POINT ( 'NONE',  ( 16.57210152137263393, -0.008007331252332796495, -0.01214401161737526519 ) ) ;
#10854 = DIRECTION ( 'NONE',  ( 0.000000000000000000, 0.000000000000000000, 1.000000000000000000 ) ) ;
#10855 = PRODUCT_CONTEXT ( 'NONE', #6076, 'mechanical' ) ;
#10856 =( LENGTH_UNIT ( ) NAMED_UNIT ( * ) SI_UNIT ( .MILLI., .METRE. ) );
#10857 = CARTESIAN_POINT ( 'NONE',  ( 3.950837973638668288, 0.000000000000000000, 0.000000000000000000 ) ) ;
#10858 = CARTESIAN_POINT ( 'NONE',  ( 16.57605080000000086, 4.769696007084728073, -1.500000000000000000 ) ) ;
#10859 = AXIS2_PLACEMENT_3D ( 'NONE', #12459, #16853, #12633 ) ;
#10860 = AXIS2_PLACEMENT_3D ( 'NONE', #12614, #6262, #14059 ) ;
#10861 = CARTESIAN_POINT ( 'NONE',  ( 1.846138399168762101, 7.646096044340033870, -9.815003036200328879 ) ) ;
#10862 = CIRCLE ( 'NONE', #14491, 5.000000000000000888 ) ;
#10863 = CARTESIAN_POINT ( 'NONE',  ( 0.3137051932979757485, 8.442169467526850823, 10.83767969834806166 ) ) ;
#10864 = B_SPLINE_CURVE_WITH_KNOTS ( 'NONE', 3,
 ( #10573, #9136, #13626, #4934, #17941, #6174, #3189, #16594, #14958, #549, #251, #4841, #7521 ),
 .UNSPECIFIED., .F., .F.,
 ( 4, 3, 3, 3, 4 ),
 ( 1.734723475976807094E-18, 0.0002299804304191480130, 0.0004599608082120234913, 0.0006467586077648008244, 0.0008336169836825994828 ),
 .UNSPECIFIED. ) ;
#10865 = CARTESIAN_POINT ( 'NONE',  ( 0.4862570985993235340, -11.67702470553359539, -7.559321496869553236 ) ) ;
#10866 = CARTESIAN_POINT ( 'NONE',  ( 8.438534575730034959, 5.688336279099046600, 3.845978796786057696 ) ) ;
#10867 = VERTEX_POINT ( 'NONE', #6573 ) ;
#10868 = EDGE_CURVE ( 'NONE', #618, #13860, #14155, .T. ) ;
#10869 = EDGE_LOOP ( 'NONE', ( #11098, #3275, #12974, #18286 ) ) ;
#10870 = ORIENTED_EDGE ( 'NONE', *, *, #4017, .F. ) ;
#10871 = VERTEX_POINT ( 'NONE', #9153 ) ;
#10872 = ORIENTED_EDGE ( 'NONE', *, *, #18361, .T. ) ;
#10873 = ADVANCED_FACE ( 'NONE', ( #10883 ), #17808, .T. ) ;
#10874 = B_SPLINE_CURVE_WITH_KNOTS ( 'NONE', 3,
 ( #10905, #1024, #3716, #13844, #6689, #5148 ),
 .UNSPECIFIED., .F., .F.,
 ( 4, 2, 4 ),
 ( 2.462833906345087556E-18, 0.0001828790815886951863, 0.0003657581631773856022 ),
 .UNSPECIFIED. ) ;
#10875 = VECTOR ( 'NONE', #15529, 1000.000000000000000 ) ;
#10876 = AXIS2_PLACEMENT_3D ( 'NONE', #14316, #1214, #18697 ) ;
#10877 = CARTESIAN_POINT ( 'NONE',  ( 0.3148213771069381384, 10.97836617636225220, 8.260246460850757089 ) ) ;
#10878 = CARTESIAN_POINT ( 'NONE',  ( -0.2640320147533066208, -7.500000000000001776, -14.20017596028259277 ) ) ;
#10879 = ORIENTED_EDGE ( 'NONE', *, *, #3522, .F. ) ;
#10880 = CARTESIAN_POINT ( 'NONE',  ( 3.950837973638676281, 2.591948120962007884, -14.31366178983250670 ) ) ;
#10881 = DIRECTION ( 'NONE',  ( -0.000000000000000000, -0.000000000000000000, -1.000000000000000000 ) ) ;
#10882 = CARTESIAN_POINT ( 'NONE',  ( -1.979226605763932723, -19.99999999999999645, 3.000000000000000000 ) ) ;
#10883 = FACE_OUTER_BOUND ( 'NONE', #8963, .T. ) ;
#10884 = LINE ( 'NONE', #833, #7582 ) ;
#10885 = CARTESIAN_POINT ( 'NONE',  ( 0.4385251269669940277, 8.732456510146231921, -10.76637725024242442 ) ) ;
#10886 = DIRECTION ( 'NONE',  ( 0.000000000000000000, 0.000000000000000000, -1.000000000000000000 ) ) ;
#10887 = ORIENTED_EDGE ( 'NONE', *, *, #15898, .F. ) ;
#10888 = VECTOR ( 'NONE', #2812, 1000.000000000000000 ) ;
#10889 = STYLED_ITEM ( 'NONE', ( #2066 ), #5561 ) ;
#10890 = ORIENTED_EDGE ( 'NONE', *, *, #16666, .F. ) ;
#10891 = ORIENTED_EDGE ( 'NONE', *, *, #17354, .T. ) ;
#10892 = ORIENTED_EDGE ( 'NONE', *, *, #7083, .T. ) ;
#10893 = CARTESIAN_POINT ( 'NONE',  ( 3.074695600507134419, -7.366518011945905720, -13.70113613813221676 ) ) ;
#10894 = EDGE_CURVE ( 'NONE', #14601, #11623, #7338, .T. ) ;
#10895 = EDGE_CURVE ( 'NONE', #13902, #10123, #14436, .T. ) ;
#10896 = EDGE_CURVE ( 'NONE', #8069, #16711, #1932, .T. ) ;
#10897 = CARTESIAN_POINT ( 'NONE',  ( 16.56872352241294521, 0.001821578298043785094, -0.01027347319884367241 ) ) ;
#10898 = CARTESIAN_POINT ( 'NONE',  ( 0.8740764193772003754, 13.83508774436055511, -3.609949042658134211 ) ) ;
#10899 = DIRECTION ( 'NONE',  ( 0.000000000000000000, 0.000000000000000000, -1.000000000000000000 ) ) ;
#10900 = CARTESIAN_POINT ( 'NONE',  ( 1.846138399168762989, 9.815003036200414144, 7.646096044339929954 ) ) ;
#10901 = EDGE_LOOP ( 'NONE', ( #18875, #12109, #553 ) ) ;
#10902 = FACE_OUTER_BOUND ( 'NONE', #5000, .T. ) ;
#10903 = CARTESIAN_POINT ( 'NONE',  ( 0.4862570985993235340, 7.559321496869426227, 11.67702470553367711 ) ) ;
#10904 = CARTESIAN_POINT ( 'NONE',  ( -1.149970134828562696, 6.907561563897650636, -11.99999999384793270 ) ) ;
#10905 = CARTESIAN_POINT ( 'NONE',  ( 1.846138399168762101, -7.646096044339961040, 9.815003036200383946 ) ) ;
#10906 = COLOUR_RGB ( '', 0.72549020, 0.75294118, 0.79215686) ;
#10907 = DIRECTION ( 'NONE',  ( -0.000000000000000000, -0.000000000000000000, -1.000000000000000000 ) ) ;
#10908 = DIRECTION ( 'NONE',  ( -1.000000000000000000, -0.000000000000000000, -0.000000000000000000 ) ) ;
#10909 = EDGE_CURVE ( 'NONE', #14561, #15826, #2968, .T. ) ;
#10910 = VERTEX_POINT ( 'NONE', #9788 ) ;
#10912 = ORIENTED_EDGE ( 'NONE', *, *, #9112, .T. ) ;
#10911 = CARTESIAN_POINT ( 'NONE',  ( 16.57210152137263393, 0.01136813053532075186, 0.009075239946108242667 ) ) ;
#10913 = CARTESIAN_POINT ( 'NONE',  ( 3.950837973638677170, 6.316429227969654114, -13.10350451991833687 ) ) ;
#10914 = AXIS2_PLACEMENT_3D ( 'NONE', #6557, #12377, #15332 ) ;
#10915 =( GEOMETRIC_REPRESENTATION_CONTEXT ( 3 ) GLOBAL_UNCERTAINTY_ASSIGNED_CONTEXT ( ( #6915 ) ) GLOBAL_UNIT_ASSIGNED_CONTEXT ( ( #15055, #13996, #1973 ) ) REPRESENTATION_CONTEXT ( 'NONE', 'WORKASPACE' ) );
#10916 = AXIS2_PLACEMENT_3D ( 'NONE', #17860, #18723, #274 ) ;
#10917 = B_SPLINE_CURVE_WITH_KNOTS ( 'NONE', 3,
 ( #5910, #4210, #5528, #7367, #4497, #14612, #10027, #3031, #17483, #11565, #2749, #8879, #11658 ),
 .UNSPECIFIED., .F., .F.,
 ( 4, 3, 3, 3, 4 ),
 ( 3.878959614448864246E-18, 0.0002299780670421054142, 0.0004599561239687919093, 0.0006896788984287899067, 0.0009194956271626406052 ),
 .UNSPECIFIED. ) ;
#10918 = ORIENTED_EDGE ( 'NONE', *, *, #13718, .F. ) ;
#10919 = CARTESIAN_POINT ( 'NONE',  ( 1.847380140988743591, -3.949801494731685292, -11.79969976631075390 ) ) ;
#10920 = CARTESIAN_POINT ( 'NONE',  ( -1.824285781648417037, -7.500000000000000888, -15.12168601478888874 ) ) ;
#10921 = EDGE_CURVE ( 'NONE', #3029, #4457, #14195, .T. ) ;
#10922 = ORIENTED_EDGE ( 'NONE', *, *, #11488, .T. ) ;
#10923 = CARTESIAN_POINT ( 'NONE',  ( 0.4862570985993235340, -8.769551628660812170, 10.79774104611370333 ) ) ;
#10924 = DIRECTION ( 'NONE',  ( -1.000000000000000000, 0.000000000000000000, 0.000000000000000000 ) ) ;
#10925 = EDGE_CURVE ( 'NONE', #2805, #10015, #4059, .T. ) ;
#10926 = VECTOR ( 'NONE', #16413, 1000.000000000000114 ) ;
#10927 = CARTESIAN_POINT ( 'NONE',  ( 1.918918678667048461, -12.08296592096905187, -3.258447776119960615 ) ) ;
#10928 = DIRECTION ( 'NONE',  ( 1.000000000000000000, 0.000000000000000000, 0.000000000000000000 ) ) ;
#10929 = AXIS2_PLACEMENT_3D ( 'NONE', #13784, #2138, #15131 ) ;
#10930 = EDGE_CURVE ( 'NONE', #10260, #17138, #8019, .T. ) ;
#10931 = CARTESIAN_POINT ( 'NONE',  ( 2.002547531651519996, 3.242439124566821818, -12.17374746633574745 ) ) ;
#10932 =( BOUNDED_SURFACE ( )  B_SPLINE_SURFACE ( 3, 1, ( 
 ( #319, #17718 ),
 ( #9010, #2970 ),
 ( #4419, #5940 ),
 ( #13402, #17420 ) ),
 .UNSPECIFIED., .F., .F., .T. ) 
 B_SPLINE_SURFACE_WITH_KNOTS ( ( 4, 4 ),
 ( 2, 2 ),
 ( 0.000000000000000000, 1.000000000000000000 ),
 ( 0.000000000000000000, 1.000000000000000000 ),
 .UNSPECIFIED. ) 
 GEOMETRIC_REPRESENTATION_ITEM ( )  RATIONAL_B_SPLINE_SURFACE ( (
 ( 1.000000000000000000, 1.000000000000000000),
 ( 0.9933953342250438912, 0.8357391271907739227),
 ( 0.9933953342250438912, 0.8357391271907739227),
 ( 1.000000000000000000, 1.000000000000000000) ) ) 
 REPRESENTATION_ITEM ( '' )  SURFACE ( )  );
#10933 = CARTESIAN_POINT ( 'NONE',  ( 0.3137051932979809665, -3.805684345189881856, 13.20008686438104739 ) ) ;
#10935 = ORIENTED_EDGE ( 'NONE', *, *, #15449, .F. ) ;
#10934 = CARTESIAN_POINT ( 'NONE',  ( 2.002547531651519996, -11.75462648437105173, 4.532360870844282630 ) ) ;
#10936 = CARTESIAN_POINT ( 'NONE',  ( 16.58200780006414732, 0.0006320991582349651770, -0.01115192838421568376 ) ) ;
#10937 = CIRCLE ( 'NONE', #7904, 13.42403576283810906 ) ;
#10938 = ORIENTED_EDGE ( 'NONE', *, *, #16449, .F. ) ;
#10939 = CARTESIAN_POINT ( 'NONE',  ( 2.002547531651519996, 12.17374746633582561, -3.242439124566524278 ) ) ;
#10940 = CARTESIAN_POINT ( 'NONE',  ( 1.846138399168762989, 11.95493567637850774, 3.446241763653039580 ) ) ;
#10941 = VERTEX_POINT ( 'NONE', #9614 ) ;
#10942 = VERTEX_POINT ( 'NONE', #15618 ) ;
#10943 = DIRECTION ( 'NONE',  ( 1.000000000000000000, 0.000000000000000000, 0.000000000000000000 ) ) ;
#10944 = FACE_OUTER_BOUND ( 'NONE', #14302, .T. ) ;
#10945 = ORIENTED_EDGE ( 'NONE', *, *, #2090, .T. ) ;
#10946 = EDGE_CURVE ( 'NONE', #18169, #2106, #9555, .T. ) ;
#10947 = CARTESIAN_POINT ( 'NONE',  ( 16.58200780006414732, -0.01041078477703985539, 0.004047297414157853025 ) ) ;
#10948 = CARTESIAN_POINT ( 'NONE',  ( 0.4862570985993235340, -0.7479633556563419772, 13.89016912371017121 ) ) ;
#10949 = CARTESIAN_POINT ( 'NONE',  ( 12.00000000000000711, -19.99999999999999645, 7.000000000000000000 ) ) ;
#10950 = VECTOR ( 'NONE', #3360, 1000.000000000000000 ) ;
#10951 = CARTESIAN_POINT ( 'NONE',  ( 1.342453679581834924, 5.476372339890209773, -13.74702459364878315 ) ) ;
#10952 = APPLICATION_PROTOCOL_DEFINITION ( 'draft international standard', 'automotive_design', 1998, #3386 ) ;
#10953 = LINE ( 'NONE', #13892, #14118 ) ;
#10954 = CARTESIAN_POINT ( 'NONE',  ( 0.3132642857406489623, -11.41580579227782444, 7.641821025099830855 ) ) ;
#10955 = CARTESIAN_POINT ( 'NONE',  ( 16.56782317627811096, 0.009439921864426468329, 0.002708056627497651414 ) ) ;
#10956 = CARTESIAN_POINT ( 'NONE',  ( 0.3137051932979809665, 3.805684345189785933, 13.20008686438107581 ) ) ;
#10957 = EDGE_CURVE ( 'NONE', #11716, #10648, #3783, .T. ) ;
#10958 = B_SPLINE_CURVE_WITH_KNOTS ( 'NONE', 3,
 ( #5642, #6913, #18468, #7007, #8717, #5464, #11498, #12822, #3948, #5738, #14353, #1259, #15597 ),
 .UNSPECIFIED., .F., .F.,
 ( 4, 3, 3, 3, 4 ),
 ( 3.878959614448864246E-18, 0.0002299780670421063358, 0.0004599561239687880061, 0.0006896788984287903403, 0.0009194956271626402800 ),
 .UNSPECIFIED. ) ;
#10959 = CARTESIAN_POINT ( 'NONE',  ( 2.750000000000000000, 0.000000000000000000, 4.750000000000000000 ) ) ;
#10960 = DIRECTION ( 'NONE',  ( -0.7635533937278214944, 0.5095610256143914274, -0.3966532189476541514 ) ) ;
#10961 = ORIENTED_EDGE ( 'NONE', *, *, #12217, .T. ) ;
#10962 = EDGE_LOOP ( 'NONE', ( #10429, #5875, #6396, #2699 ) ) ;
#10963 = ORIENTED_EDGE ( 'NONE', *, *, #8485, .F. ) ;
#10964 = B_SPLINE_CURVE_WITH_KNOTS ( 'NONE', 3,
 ( #10733, #411, #608, #7780 ),
 .UNSPECIFIED., .F., .F.,
 ( 4, 4 ),
 ( 0.000000000000000000, 0.002004993803842712932 ),
 .UNSPECIFIED. ) ;
#10965 = ORIENTED_EDGE ( 'NONE', *, *, #2025, .F. ) ;
#10966 =( BOUNDED_SURFACE ( )  B_SPLINE_SURFACE ( 3, 1, ( 
 ( #3375, #9214 ),
 ( #15415, #12629 ),
 ( #8346, #11397 ),
 ( #15321, #16850 ) ),
 .UNSPECIFIED., .F., .F., .T. ) 
 B_SPLINE_SURFACE_WITH_KNOTS ( ( 4, 4 ),
 ( 2, 2 ),
 ( 0.000000000000000000, 1.000000000000000000 ),
 ( 0.000000000000000000, 1.000000000000000000 ),
 .UNSPECIFIED. ) 
 GEOMETRIC_REPRESENTATION_ITEM ( )  RATIONAL_B_SPLINE_SURFACE ( (
 ( 1.000000000000000000, 1.000000000000000000),
 ( 0.9933953342250438912, 0.8357391271907739227),
 ( 0.9933953342250438912, 0.8357391271907739227),
 ( 1.000000000000000000, 1.000000000000000000) ) ) 
 REPRESENTATION_ITEM ( '' )  SURFACE ( )  );
#10967 = CARTESIAN_POINT ( 'NONE',  ( 8.522092701127531811, -2.505958102592667824, 6.489356537178181838 ) ) ;
#10968 = CARTESIAN_POINT ( 'NONE',  ( 3.647233657245696925, -7.500000000000000888, -16.29053473562044019 ) ) ;
#10969 = CARTESIAN_POINT ( 'NONE',  ( 1.918921323896322750, -12.49850046818174398, -0.6349083173281465653 ) ) ;
#10970 = CARTESIAN_POINT ( 'NONE',  ( 1.846524061778021419, -11.93805390544203426, 3.506196582971057740 ) ) ;
#10971 = EDGE_CURVE ( 'NONE', #18304, #10455, #18393, .T. ) ;
#10972 = CYLINDRICAL_SURFACE ( 'NONE', #11166, 5.000000000000000888 ) ;
#10973 = DIRECTION ( 'NONE',  ( -0.000000000000000000, -0.000000000000000000, 1.000000000000000000 ) ) ;
#10974 = CARTESIAN_POINT ( 'NONE',  ( 0.8740764193769885448, -7.708542792189400750, -12.04241474978016058 ) ) ;
#10975 = AXIS2_PLACEMENT_3D ( 'NONE', #9001, #4518, #10436 ) ;
#10976 = CARTESIAN_POINT ( 'NONE',  ( 3.074695600507132198, -14.01296402267896823, -6.754521329825003306 ) ) ;
#10977 = DIRECTION ( 'NONE',  ( -2.891205793294679312E-16, -1.000000000000000000, 0.000000000000000000 ) ) ;
#10978 = EDGE_LOOP ( 'NONE', ( #4651, #17317, #9118, #14284 ) ) ;
#10979 = B_SPLINE_CURVE_WITH_KNOTS ( 'NONE', 3,
 ( #1968, #7713, #10762, #9504, #13519, #3385 ),
 .UNSPECIFIED., .F., .F.,
 ( 4, 2, 4 ),
 ( 0.000000000000000000, 0.001656992708823338926, 0.003313985417646677853 ),
 .UNSPECIFIED. ) ;
#10980 = VERTEX_POINT ( 'NONE', #18493 ) ;
#10981 = ORIENTED_EDGE ( 'NONE', *, *, #2827, .F. ) ;
#10982 = ORIENTED_EDGE ( 'NONE', *, *, #3294, .T. ) ;
#10983 = CARTESIAN_POINT ( 'NONE',  ( 0.000000000000000000, 6.799999999999999822, 0.000000000000000000 ) ) ;
#10984 = CARTESIAN_POINT ( 'NONE',  ( 3.950837973638668288, 0.000000000000000000, 0.000000000000000000 ) ) ;
#10985 = VECTOR ( 'NONE', #10212, 1000.000000000000000 ) ;
#10986 = DIRECTION ( 'NONE',  ( -0.000000000000000000, 0.5000000000000003331, -0.8660254037844384856 ) ) ;
#10987 = CARTESIAN_POINT ( 'NONE',  ( 16.57778382496167424, -0.01018821665058842162, -0.01092721432669105028 ) ) ;
#10988 = AXIS2_PLACEMENT_3D ( 'NONE', #7463, #17878, #14905 ) ;
#10989 = DIRECTION ( 'NONE',  ( -0.000000000000000000, -0.000000000000000000, 1.000000000000000000 ) ) ;
#10990 = ORIENTED_EDGE ( 'NONE', *, *, #10296, .T. ) ;
#10991 = AXIS2_PLACEMENT_3D ( 'NONE', #12339, #12520, #15484 ) ;
#10992 = CARTESIAN_POINT ( 'NONE',  ( 2.320521194581854907, 15.64520804578206281, -1.795798718312993758 ) ) ;
#10993 = CARTESIAN_POINT ( 'NONE',  ( 1.847168016377984889, -11.89018175117591980, -3.666915430942724097 ) ) ;
#10994 = B_SPLINE_CURVE_WITH_KNOTS ( 'NONE', 3,
 ( #13371, #13559, #16244, #3425 ),
 .UNSPECIFIED., .F., .F.,
 ( 4, 4 ),
 ( 0.000000000000000000, 0.002004993803841946618 ),
 .UNSPECIFIED. ) ;
#10995 = CARTESIAN_POINT ( 'NONE',  ( 0.5119965487701979567, 7.499999999999962697, -13.04039602617943672 ) ) ;
#10996 = DIRECTION ( 'NONE',  ( 0.000000000000000000, 0.000000000000000000, 1.000000000000000000 ) ) ;
#10997 = DIRECTION ( 'NONE',  ( -1.000000000000000000, 0.000000000000000000, 0.000000000000000000 ) ) ;
#10998 = PRESENTATION_STYLE_ASSIGNMENT (( #2017 ) ) ;
#10999 = CARTESIAN_POINT ( 'NONE',  ( 2.369999999999999662, 0.000000000000000000, 0.000000000000000000 ) ) ;
#11000 = CARTESIAN_POINT ( 'NONE',  ( 1.845755665166727066, -4.296872077620760066, 11.67596932341233007 ) ) ;
#11001 = EDGE_CURVE ( 'NONE', #8116, #8373, #16452, .T. ) ;
#11002 = EDGE_LOOP ( 'NONE', ( #5956, #11010, #15494, #12515 ) ) ;
#11004 = ORIENTED_EDGE ( 'NONE', *, *, #9238, .T. ) ;
#11003 = DIRECTION ( 'NONE',  ( 0.7635533937278216055, 0.3966532189476633663, -0.5095610256143844330 ) ) ;
#11005 = DIRECTION ( 'NONE',  ( 0.000000000000000000, 0.000000000000000000, 1.000000000000000000 ) ) ;
#11006 = CARTESIAN_POINT ( 'NONE',  ( 16.56753206892534891, 0.009389754735541551434, -0.001421777558676823056 ) ) ;
#11007 = VERTEX_POINT ( 'NONE', #8555 ) ;
#11008 = FACE_OUTER_BOUND ( 'NONE', #86, .T. ) ;
#11009 = CARTESIAN_POINT ( 'NONE',  ( -4.238775304281396927, -7.500000000000402345, -13.18441022661327011 ) ) ;
#11010 = ORIENTED_EDGE ( 'NONE', *, *, #8602, .T. ) ;
#11011 = CARTESIAN_POINT ( 'NONE',  ( 1.846138399168762101, -6.971848976711082280, 10.30487220521567693 ) ) ;
#11012 = CARTESIAN_POINT ( 'NONE',  ( 0.4385251269669947494, -13.39302348765811068, 3.577373010348662508 ) ) ;
#11013 = CARTESIAN_POINT ( 'NONE',  ( 0.3137051932979757485, 7.698472063774634222, -11.37800749014122736 ) ) ;
#11014 = CYLINDRICAL_SURFACE ( 'NONE', #7179, 5.000000000000004441 ) ;
#11015 = AXIS2_PLACEMENT_3D ( 'NONE', #5376, #12364, #18197 ) ;
#11016 = ADVANCED_FACE ( 'NONE', ( #11249 ), #7240, .F. ) ;
#11017 = ADVANCED_FACE ( 'NONE', ( #17067 ), #13087, .F. ) ;
#11018 = CARTESIAN_POINT ( 'NONE',  ( 0.4862570985993235340, 3.580942890621860109, -13.44146924561377254 ) ) ;
#11019 = ADVANCED_FACE ( 'NONE', ( #2617 ), #8465, .T. ) ;
#11020 = CARTESIAN_POINT ( 'NONE',  ( 16.56872352241294521, -0.009382111268607402216, -0.004564908236399935551 ) ) ;
#11022 = VERTEX_POINT ( 'NONE', #8645 ) ;
#11021 = CARTESIAN_POINT ( 'NONE',  ( 0.4862570985993235340, -11.67702470553370553, 7.559321496869385371 ) ) ;
#11023 = CARTESIAN_POINT ( 'NONE',  ( 8.522092701127531811, 2.505958102592620751, 6.489356537178200490 ) ) ;
#11024 = CARTESIAN_POINT ( 'NONE',  ( 16.56782317627811096, -0.007739510688079557534, -0.006045301465876337828 ) ) ;
#11025 = CARTESIAN_POINT ( 'NONE',  ( 0.3150692679895942816, -11.02465386701222805, -8.199139630396127032 ) ) ;
#11026 = CARTESIAN_POINT ( 'NONE',  ( -27.50000000000000711, -12.50000000000000178, 0.000000000000000000 ) ) ;
#11027 = B_SPLINE_CURVE_WITH_KNOTS ( 'NONE', 3,
 ( #1948, #699, #13499, #3656 ),
 .UNSPECIFIED., .F., .F.,
 ( 4, 4 ),
 ( 1.734723475976807094E-17, 0.003005512676784844427 ),
 .UNSPECIFIED. ) ;
#11028 = ORIENTED_EDGE ( 'NONE', *, *, #8809, .F. ) ;
#11029 = ORIENTED_EDGE ( 'NONE', *, *, #623, .F. ) ;
#11030 = CARTESIAN_POINT ( 'NONE',  ( 3.074695600507132198, -14.01296402267896823, -6.754521329825003306 ) ) ;
#11031 = DIRECTION ( 'NONE',  ( 1.000000000000000000, 1.734723475976806848E-16, 0.000000000000000000 ) ) ;
#11032 = VERTEX_POINT ( 'NONE', #4446 ) ;
#11033 = CARTESIAN_POINT ( 'NONE',  ( 16.57778382496167424, -0.01482878558584568157, -0.001819584982832054632 ) ) ;
#11034 = CARTESIAN_POINT ( 'NONE',  ( 1.845756295923359769, 10.33914852636104875, 6.920504327368230513 ) ) ;
#11035 = AXIS2_PLACEMENT_3D ( 'NONE', #10999, #10908, #3629 ) ;
#11036 = CARTESIAN_POINT ( 'NONE',  ( 0.4754618798421171855, -11.68486377711960778, -7.564402563418600067 ) ) ;
#11037 = B_SPLINE_CURVE_WITH_KNOTS ( 'NONE', 3,
 ( #18624, #5527, #15759, #17780, #3427, #6117, #482, #14994, #6406, #14804, #13272, #288, #10800 ),
 .UNSPECIFIED., .F., .F.,
 ( 4, 3, 3, 3, 4 ),
 ( 2.168404344971008868E-18, 0.0002299804304191472269, 0.0004599608082120226239, 0.0006467586077647999570, 0.0008336169836825976396 ),
 .UNSPECIFIED. ) ;
#11038 = CARTESIAN_POINT ( 'NONE',  ( 0.8740764193767192047, -0.8420116711622469552, 14.27348595579779911 ) ) ;
#11039 = FACE_OUTER_BOUND ( 'NONE', #9530, .T. ) ;
#11040 = CARTESIAN_POINT ( 'NONE',  ( 0.8740779401508862456, -13.31469722824359891, 5.211551231203810808 ) ) ;
#11041 = ITEM_DEFINED_TRANSFORMATION ( 'NONE', 'NONE', #533,  #2030 ) ;
#11042 =( BOUNDED_SURFACE ( )  B_SPLINE_SURFACE ( 3, 1, ( 
 ( #11020, #14340 ),
 ( #9941, #15770 ),
 ( #14062, #5452 ),
 ( #3932, #1153 ) ),
 .UNSPECIFIED., .F., .F., .T. ) 
 B_SPLINE_SURFACE_WITH_KNOTS ( ( 4, 4 ),
 ( 2, 2 ),
 ( 0.000000000000000000, 1.000000000000000000 ),
 ( 0.000000000000000000, 1.000000000000000000 ),
 .UNSPECIFIED. ) 
 GEOMETRIC_REPRESENTATION_ITEM ( )  RATIONAL_B_SPLINE_SURFACE ( (
 ( 1.000000000000000000, 1.000000000000000000),
 ( 0.7792777138730160313, 0.9689936506012927220),
 ( 0.7792777138730160313, 0.9689936506012927220),
 ( 1.000000000000000000, 1.000000000000000000) ) ) 
 REPRESENTATION_ITEM ( '' )  SURFACE ( )  );
#11043 = CARTESIAN_POINT ( 'NONE',  ( 2.002547531651519996, 7.942910686618313676, -9.778737580845612953 ) ) ;
#11044 = CARTESIAN_POINT ( 'NONE',  ( 3.950837973638675393, -2.591948120961912849, 14.31366178983252446 ) ) ;
#11045 = B_SPLINE_CURVE_WITH_KNOTS ( 'NONE', 3,
 ( #9269, #1530, #98, #5912, #11757, #4499 ),
 .UNSPECIFIED., .F., .F.,
 ( 4, 2, 4 ),
 ( 4.027530160694267299E-17, 0.0002014099069817290014, 0.0004028198139634177246 ),
 .UNSPECIFIED. ) ;
#11046 = CARTESIAN_POINT ( 'NONE',  ( 16.56822296793089322, 0.009385634690641620620, 0.003834730849370876320 ) ) ;
#11047 = CARTESIAN_POINT ( 'NONE',  ( 2.002547531651519996, -9.778737580845639599, -7.942910686618280813 ) ) ;
#11048 = B_SPLINE_CURVE_WITH_KNOTS ( 'NONE', 3,
 ( #4144, #11135, #1266, #18656, #11505, #15604 ),
 .UNSPECIFIED., .F., .F.,
 ( 4, 2, 4 ),
 ( 0.000000000000000000, 0.0002017457492448075543, 0.0004034914984896151085 ),
 .UNSPECIFIED. ) ;
#11049 = CIRCLE ( 'NONE', #16835, 0.5000000000000004441 ) ;
#11050 = EDGE_CURVE ( 'NONE', #4529, #12695, #8670, .T. ) ;
#11051 = FACE_OUTER_BOUND ( 'NONE', #12249, .T. ) ;
#11052 = ORIENTED_EDGE ( 'NONE', *, *, #8315, .T. ) ;
#11053 = VERTEX_POINT ( 'NONE', #13042 ) ;
#11054 = EDGE_LOOP ( 'NONE', ( #10578, #13632, #12744, #18501, #4538, #16577, #12107, #6449, #2386, #4958, #5138, #9445, #8868, #14064, #10982, #14503, #6226, #4632, #2360, #1584, #14515, #14459, #17429, #3318, #15846, #499, #12800, #5655, #2880, #9088, #6447, #14328, #5676, #10216, #12487, #13980, #6084, #14803, #6685, #17130, #708, #15255, #6807, #6445, #1219, #6159, #5748, #5460, #17073, #10409, #9168, #3622, #9551, #4356, #7647, #15412, #2440, #12400, #17821, #3426, #11531, #8288, #924, #17953 ) ) ;
#11055 = ORIENTED_EDGE ( 'NONE', *, *, #6124, .F. ) ;
#11056 = CARTESIAN_POINT ( 'NONE',  ( 2.002547531651519996, -9.778737580845755062, 7.942910686618138705 ) ) ;
#11057 = CARTESIAN_POINT ( 'NONE',  ( -2.066926351139552143, -7.500000000000001776, -15.30321684074790234 ) ) ;
#11058 = B_SPLINE_CURVE_WITH_KNOTS ( 'NONE', 3,
 ( #15518, #13995, #9422, #2074, #15333, #17053 ),
 .UNSPECIFIED., .F., .F.,
 ( 4, 2, 4 ),
 ( 5.421010862427522170E-19, 0.0001825746017570580189, 0.0003651492035141154957 ),
 .UNSPECIFIED. ) ;
#11059 = CARTESIAN_POINT ( 'NONE',  ( 1.861628059977342264, -3.332996951203546665, -12.00316790821105073 ) ) ;
#11060 = FACE_BOUND ( 'NONE', #10458, .T. ) ;
#11061 = CARTESIAN_POINT ( 'NONE',  ( 0.000000000000000000, 0.000000000000000000, 10.00000000000000000 ) ) ;
#11062 = CARTESIAN_POINT ( 'NONE',  ( 3.512766787570877902, 13.25664064834461264, 7.127386085302796381 ) ) ;
#11063 = FACE_OUTER_BOUND ( 'NONE', #7231, .T. ) ;
#11064 = PRODUCT_RELATED_PRODUCT_CATEGORY ( 'part', '', ( #7708 ) ) ;
#11065 = AXIS2_PLACEMENT_3D ( 'NONE', #3821, #5346, #9647 ) ;
#11066 = EDGE_CURVE ( 'NONE', #9395, #16458, #5768, .T. ) ;
#11067 = FACE_OUTER_BOUND ( 'NONE', #4311, .T. ) ;
#11068 = LINE ( 'NONE', #5225, #14865 ) ;
#11069 = ORIENTED_EDGE ( 'NONE', *, *, #2377, .F. ) ;
#11070 = ADVANCED_FACE ( 'NONE', ( #16303 ), #10272, .T. ) ;
#11071 = ORIENTED_EDGE ( 'NONE', *, *, #6712, .F. ) ;
#11072 = ORIENTED_EDGE ( 'NONE', *, *, #18161, .F. ) ;
#11073 = ORIENTED_EDGE ( 'NONE', *, *, #3713, .T. ) ;
#11074 =( BOUNDED_SURFACE ( )  B_SPLINE_SURFACE ( 3, 1, ( 
 ( #8300, #6686 ),
 ( #16808, #13754 ),
 ( #11082, #8031 ),
 ( #18151, #13933 ) ),
 .UNSPECIFIED., .F., .F., .T. ) 
 B_SPLINE_SURFACE_WITH_KNOTS ( ( 4, 4 ),
 ( 2, 2 ),
 ( 0.000000000000000000, 1.000000000000000000 ),
 ( 0.000000000000000000, 1.000000000000000000 ),
 .UNSPECIFIED. ) 
 GEOMETRIC_REPRESENTATION_ITEM ( )  RATIONAL_B_SPLINE_SURFACE ( (
 ( 1.000000000000000000, 1.000000000000000000),
 ( 0.7792777138730160313, 0.9689936506012927220),
 ( 0.7792777138730160313, 0.9689936506012927220),
 ( 1.000000000000000000, 1.000000000000000000) ) ) 
 REPRESENTATION_ITEM ( '' )  SURFACE ( )  );
#11075 = LINE ( 'NONE', #5320, #17859 ) ;
#11076 = DIRECTION ( 'NONE',  ( 0.000000000000000000, -0.8660254037844384856, 0.5000000000000004441 ) ) ;
#11077 = CARTESIAN_POINT ( 'NONE',  ( -20.00000000000000000, -2.500000000000000444, -17.00000000000000000 ) ) ;
#11078 = B_SPLINE_CURVE_WITH_KNOTS ( 'NONE', 3,
 ( #10128, #1239, #2841, #8692, #11661, #7079 ),
 .UNSPECIFIED., .F., .F.,
 ( 4, 2, 4 ),
 ( 4.023840028577795923E-17, 0.0002014099069817275377, 0.0004028198139634147973 ),
 .UNSPECIFIED. ) ;
#11079 = CARTESIAN_POINT ( 'NONE',  ( 8.522092701127531811, -0.3779863304870734741, -6.946128462138600135 ) ) ;
#11080 = CARTESIAN_POINT ( 'NONE',  ( 1.846524061778018977, -7.597197846158149304, 9.853584647934361840 ) ) ;
#11081 = ORIENTED_EDGE ( 'NONE', *, *, #6662, .F. ) ;
#11082 = CARTESIAN_POINT ( 'NONE',  ( 16.57778382496167424, 0.007244066302947695102, -0.01306626476309380794 ) ) ;
#11083 = EDGE_CURVE ( 'NONE', #12603, #15726, #5873, .T. ) ;
#11084 = CARTESIAN_POINT ( 'NONE',  ( 6.538348415311014072, -2.500000000000000444, -17.00000000000000000 ) ) ;
#11085 = CARTESIAN_POINT ( 'NONE',  ( -2.048748540252033123, 6.701137625570393830, -11.99999999225504510 ) ) ;
#11086 = CARTESIAN_POINT ( 'NONE',  ( 3.512766787570793969, 2.682019731918377836, 14.81029789862155255 ) ) ;
#11087 =( GEOMETRIC_REPRESENTATION_CONTEXT ( 3 ) GLOBAL_UNCERTAINTY_ASSIGNED_CONTEXT ( ( #12635 ) ) GLOBAL_UNIT_ASSIGNED_CONTEXT ( ( #8265, #2327, #13889 ) ) REPRESENTATION_CONTEXT ( 'NONE', 'WORKASPACE' ) );
#11088 = CARTESIAN_POINT ( 'NONE',  ( -194.9999999999999716, -5.000000000000024869, 3.000000000000002665 ) ) ;
#11089 = LINE ( 'NONE', #5059, #9870 ) ;
#11090 = CARTESIAN_POINT ( 'NONE',  ( 0.3145729642390390768, 12.96842777670212676, -4.535980493004950986 ) ) ;
#11091 = FACE_OUTER_BOUND ( 'NONE', #15139, .T. ) ;
#11092 = ORIENTED_EDGE ( 'NONE', *, *, #8033, .T. ) ;
#11093 = ORIENTED_EDGE ( 'NONE', *, *, #14523, .T. ) ;
#11094 = CARTESIAN_POINT ( 'NONE',  ( 2.747332970342022840, 16.12459247543626617, 2.705255688517901103 ) ) ;
#11095 = DIRECTION ( 'NONE',  ( -1.000000000000000000, 0.000000000000000000, 0.000000000000000000 ) ) ;
#11096 = EDGE_CURVE ( 'NONE', #15892, #9201, #14391, .T. ) ;
#11097 = AXIS2_PLACEMENT_3D ( 'NONE', #12373, #9503, #3582 ) ;
#11098 = ORIENTED_EDGE ( 'NONE', *, *, #13421, .T. ) ;
#11099 = CARTESIAN_POINT ( 'NONE',  ( 8.522092701127531811, -6.489356537178172957, -2.505958102592690473 ) ) ;
#11100 = CARTESIAN_POINT ( 'NONE',  ( -5.856338620593649402, -7.500000000000000000, -12.72522090842701736 ) ) ;
#11101 = ORIENTED_EDGE ( 'NONE', *, *, #9889, .F. ) ;
#11102 = CARTESIAN_POINT ( 'NONE',  ( 3.512766787570752669, -14.91422000116822311, 2.025881399556336060 ) ) ;
#11103 = EDGE_CURVE ( 'NONE', #14649, #998, #3444, .T. ) ;
#11104 = PLANE ( 'NONE',  #7945 ) ;
#11105 = CARTESIAN_POINT ( 'NONE',  ( 0.3132635586635982849, 7.641727604904055227, -11.41586812343481583 ) ) ;
#11106 = CARTESIAN_POINT ( 'NONE',  ( 20.00000000000000000, 0.000000000000000000, -22.00000000000000000 ) ) ;
#11107 = CARTESIAN_POINT ( 'NONE',  ( 1.959283090834840202, 7.909254450749005017, 9.750336807931171634 ) ) ;
#11108 = AXIS2_PLACEMENT_3D ( 'NONE', #4523, #18849, #18747 ) ;
#11109 = SURFACE_STYLE_USAGE ( .BOTH. , #7080 ) ;
#11110 = CARTESIAN_POINT ( 'NONE',  ( 0.4862570985993235340, -0.7479633556561480212, -13.89016912371018186 ) ) ;
#11111 = CARTESIAN_POINT ( 'NONE',  ( 16.56679352167444819, -0.006618561353599251677, 0.006526964904752932846 ) ) ;
#11113 = ORIENTED_EDGE ( 'NONE', *, *, #7745, .F. ) ;
#11112 = DIRECTION ( 'NONE',  ( 0.000000000000000000, 0.000000000000000000, 1.000000000000000000 ) ) ;
#11114 = CARTESIAN_POINT ( 'NONE',  ( 3.950837973638675393, -6.888253895133384930, 12.81214529934972823 ) ) ;
#11115 = CARTESIAN_POINT ( 'NONE',  ( 0.3151926232592488497, -11.16039997398647365, -8.013596737356504462 ) ) ;
#11116 = CARTESIAN_POINT ( 'NONE',  ( 1.845755665166724846, 4.296872077620840891, -11.67596932341229987 ) ) ;
#11117 = EDGE_LOOP ( 'NONE', ( #14489, #8581, #1978, #10344 ) ) ;
#11118 = ORIENTED_EDGE ( 'NONE', *, *, #7501, .F. ) ;
#11119 = DIRECTION ( 'NONE',  ( 0.4246593920385850485, 0.1376957914266804250, -0.8948208031649687033 ) ) ;
#11120 = CARTESIAN_POINT ( 'NONE',  ( 0.000000000000000000, 0.000000000000000000, 11.00000000000000000 ) ) ;
#11121 = ORIENTED_EDGE ( 'NONE', *, *, #13472, .F. ) ;
#11122 = CARTESIAN_POINT ( 'NONE',  ( 0.3145729642390391878, -8.321438378985172690, -10.93201268464381748 ) ) ;
#11123 = ADVANCED_FACE ( 'NONE', ( #14859 ), #15049, .F. ) ;
#11124 = EDGE_CURVE ( 'NONE', #11848, #16458, #9249, .T. ) ;
#11125 = ADVANCED_FACE ( 'NONE', ( #14569 ), #3939, .F. ) ;
#11126 = CARTESIAN_POINT ( 'NONE',  ( 1.959283090834841090, 6.829027319138399221, -10.53516775895152691 ) ) ;
#11127 = AXIS2_PLACEMENT_3D ( 'NONE', #4754, #5990, #4851 ) ;
#11128 = DIRECTION ( 'NONE',  ( -0.9034263296138832500, 0.000000000000000000, -0.4287433579198481337 ) ) ;
#11129 = CARTESIAN_POINT ( 'NONE',  ( 0.4384471787762798112, -7.540925784514636909, 11.63197976518326371 ) ) ;
#11130 = CARTESIAN_POINT ( 'NONE',  ( 1.846955891736116184, 7.525208385419960067, 9.909315188408065467 ) ) ;
#11131 = APPLICATION_PROTOCOL_DEFINITION ( 'draft international standard', 'automotive_design', 1998, #12539 ) ;
#11132 = DIRECTION ( 'NONE',  ( -1.000000000000000000, -0.000000000000000000, -0.000000000000000000 ) ) ;
#11133 = ORIENTED_EDGE ( 'NONE', *, *, #6278, .F. ) ;
#11134 = EDGE_CURVE ( 'NONE', #14697, #9064, #15512, .T. ) ;
#11135 = CARTESIAN_POINT ( 'NONE',  ( 0.3132635586635980074, -10.79541209008109703, 8.495712071659360376 ) ) ;
#11136 = CARTESIAN_POINT ( 'NONE',  ( 3.950837973638675393, 10.51028938476217967, 10.05648675950130233 ) ) ;
#11137 = FACE_OUTER_BOUND ( 'NONE', #5617, .T. ) ;
#11138 = CARTESIAN_POINT ( 'NONE',  ( 16.57778382496167424, -0.01466529584256786797, -0.002851818597093949692 ) ) ;
#11139 = ORIENTED_EDGE ( 'NONE', *, *, #9413, .T. ) ;
#11140 = VECTOR ( 'NONE', #12139, 1000.000000000000000 ) ;
#11141 = ORIENTED_EDGE ( 'NONE', *, *, #12931, .F. ) ;
#11142 = AXIS2_PLACEMENT_3D ( 'NONE', #10984, #843, #2102 ) ;
#11143 = ORIENTED_EDGE ( 'NONE', *, *, #5194, .T. ) ;
#11144 = ORIENTED_EDGE ( 'NONE', *, *, #15998, .F. ) ;
#11145 = DIRECTION ( 'NONE',  ( 0.000000000000000000, -1.000000000000000000, 0.000000000000000000 ) ) ;
#11146 =( BOUNDED_SURFACE ( )  B_SPLINE_SURFACE ( 3, 1, ( 
 ( #16114, #8847 ),
 ( #11278, #1580 ),
 ( #12598, #5342 ),
 ( #9814, #2457 ) ),
 .UNSPECIFIED., .F., .F., .T. ) 
 B_SPLINE_SURFACE_WITH_KNOTS ( ( 4, 4 ),
 ( 2, 2 ),
 ( 0.000000000000000000, 1.000000000000000000 ),
 ( 0.000000000000000000, 1.000000000000000000 ),
 .UNSPECIFIED. ) 
 GEOMETRIC_REPRESENTATION_ITEM ( )  RATIONAL_B_SPLINE_SURFACE ( (
 ( 1.000000000000000000, 1.000000000000000000),
 ( 0.9933953342250438912, 0.8357391271907739227),
 ( 0.9933953342250438912, 0.8357391271907739227),
 ( 1.000000000000000000, 1.000000000000000000) ) ) 
 REPRESENTATION_ITEM ( '' )  SURFACE ( )  );
#11147 = CARTESIAN_POINT ( 'NONE',  ( -55.93192566395838128, 9.999999999999973355, 6.000000000000000000 ) ) ;
#11148 = B_SPLINE_CURVE_WITH_KNOTS ( 'NONE', 3,
 ( #6072, #142, #4546, #17443 ),
 .UNSPECIFIED., .F., .F.,
 ( 4, 4 ),
 ( 1.811104479740059440E-17, 0.003005512676784850932 ),
 .UNSPECIFIED. ) ;
#11149 = ADVANCED_FACE ( 'NONE', ( #8929 ), #14757, .T. ) ;
#11150 = CIRCLE ( 'NONE', #10224, 5.000000000000049738 ) ;
#11151 = CARTESIAN_POINT ( 'NONE',  ( 2.636624412716062960, -2.161493821598612808, -15.91454522070331912 ) ) ;
#11152 = CARTESIAN_POINT ( 'NONE',  ( 4.176146106109656457E-15, -16.60000000000000142, 29.01316734529526187 ) ) ;
#11153 = VECTOR ( 'NONE', #17201, 1000.000000000000000 ) ;
#11154 = VECTOR ( 'NONE', #16345, 1000.000000000000114 ) ;
#11155 = CARTESIAN_POINT ( 'NONE',  ( -66.35602477868049220, -10.00000000000000888, 3.000000000000002665 ) ) ;
#11156 = CARTESIAN_POINT ( 'NONE',  ( 16.56679352167444819, -0.009170718284672552470, -0.001518074900130618379 ) ) ;
#11157 = DIRECTION ( 'NONE',  ( -0.7635533937278214944, 0.3966532189476597581, 0.5095610256143870975 ) ) ;
#11158 = CARTESIAN_POINT ( 'NONE',  ( 0.3058872367615230181, -12.87003593440631732, 4.821066432589277362 ) ) ;
#11159 = DIRECTION ( 'NONE',  ( 0.000000000000000000, 0.000000000000000000, 1.000000000000000000 ) ) ;
#11160 = EDGE_CURVE ( 'NONE', #9233, #2882, #6206, .T. ) ;
#11161 = ORIENTED_EDGE ( 'NONE', *, *, #10399, .T. ) ;
#11162 = ORIENTED_EDGE ( 'NONE', *, *, #7643, .F. ) ;
#11163 = ORIENTED_EDGE ( 'NONE', *, *, #15765, .F. ) ;
#11164 = AXIS2_PLACEMENT_3D ( 'NONE', #3380, #13423, #3578 ) ;
#11165 = ORIENTED_EDGE ( 'NONE', *, *, #4185, .T. ) ;
#11166 = AXIS2_PLACEMENT_3D ( 'NONE', #5130, #8011, #10781 ) ;
#11167 = FACE_OUTER_BOUND ( 'NONE', #572, .T. ) ;
#11168 = CARTESIAN_POINT ( 'NONE',  ( 3.664313757352974488, -12.97355833021536498, -5.926151963190507743 ) ) ;
#11169 = CARTESIAN_POINT ( 'NONE',  ( 3.950837973638677170, 10.51028938476232355, -10.05648675950114956 ) ) ;
#11170 = DIRECTION ( 'NONE',  ( -1.000000000000000000, 0.000000000000000000, 0.000000000000000000 ) ) ;
#11171 = CARTESIAN_POINT ( 'NONE',  ( 1.846613052777651198, -7.035606253495386930, 10.26230975746757146 ) ) ;
#11172 = VERTEX_POINT ( 'NONE', #541 ) ;
#11173 = CARTESIAN_POINT ( 'NONE',  ( 0.4862570985993235340, 13.89016912371017476, -0.7479633556562934604 ) ) ;
#11174 = B_SPLINE_CURVE_WITH_KNOTS ( 'NONE', 3,
 ( #5485, #8193, #12757, #6841, #11336, #18492 ),
 .UNSPECIFIED., .F., .F.,
 ( 4, 2, 4 ),
 ( 0.000000000000000000, 0.0001828790815886947255, 0.0003657581631773894511 ),
 .UNSPECIFIED. ) ;
#11175 = DIRECTION ( 'NONE',  ( 1.000000000000000000, 0.000000000000000000, 0.000000000000000000 ) ) ;
#11176 = CARTESIAN_POINT ( 'NONE',  ( 6.500003738483226989, 7.499999999998957279, -12.10028435765586252 ) ) ;
#11177 = CARTESIAN_POINT ( 'NONE',  ( 3.074695600507311610, 2.772091048739249164, 15.30693405987785916 ) ) ;
#11178 = DIRECTION ( 'NONE',  ( -1.000000000000000000, -0.000000000000000000, -0.000000000000000000 ) ) ;
#11179 = CARTESIAN_POINT ( 'NONE',  ( 0.000000000000000000, 0.000000000000000000, -12.00000000000000000 ) ) ;
#11180 = CARTESIAN_POINT ( 'NONE',  ( 16.56679352167444819, 0.008311568981097982450, 0.004162264567718830001 ) ) ;
#11181 = CIRCLE ( 'NONE', #4157, 5.000000000000004441 ) ;
#11182 = PRESENTATION_LAYER_ASSIGNMENT (  '', '', ( #13907 ) ) ;
#11183 = EDGE_CURVE ( 'NONE', #15858, #16388, #3430, .T. ) ;
#11184 = LINE ( 'NONE', #5246, #9104 ) ;
#11185 = VERTEX_POINT ( 'NONE', #9221 ) ;
#11186 =( BOUNDED_SURFACE ( )  B_SPLINE_SURFACE ( 3, 1, ( 
 ( #4705, #16271 ),
 ( #10820, #3352 ),
 ( #506, #1937 ),
 ( #6335, #17993 ) ),
 .UNSPECIFIED., .F., .F., .F. ) 
 B_SPLINE_SURFACE_WITH_KNOTS ( ( 4, 4 ),
 ( 2, 2 ),
 ( 0.000000000000000000, 1.000000000000000000 ),
 ( 0.000000000000000000, 1.000000000000000000 ),
 .UNSPECIFIED. ) 
 GEOMETRIC_REPRESENTATION_ITEM ( )  RATIONAL_B_SPLINE_SURFACE ( (
 ( 1.000000000000000000, 1.000000000000000000),
 ( 0.7792777138730160313, 0.9689936506012927220),
 ( 0.7792777138730160313, 0.9689936506012927220),
 ( 1.000000000000000000, 1.000000000000000000) ) ) 
 REPRESENTATION_ITEM ( '' )  SURFACE ( )  );
#11188 = ORIENTED_EDGE ( 'NONE', *, *, #6552, .T. ) ;
#11187 = CARTESIAN_POINT ( 'NONE',  ( 3.686287386450715076E-15, -16.60000000000000142, 25.01316734529526187 ) ) ;
#11189 = CARTESIAN_POINT ( 'NONE',  ( 16.57778382496167424, 0.006312874906843677844, -0.01354073047775769707 ) ) ;
#11190 = EDGE_CURVE ( 'NONE', #18880, #7816, #12591, .T. ) ;
#11191 = DIRECTION ( 'NONE',  ( -1.000000000000000000, 0.000000000000000000, 0.000000000000000000 ) ) ;
#11192 = ORIENTED_EDGE ( 'NONE', *, *, #17252, .F. ) ;
#11193 = CARTESIAN_POINT ( 'NONE',  ( 1.847412631396507576, -3.804043368582581408, -11.84727953344286888 ) ) ;
#11194 = CONICAL_SURFACE ( 'NONE', #16061, 14.54644660717763927, 0.8559913436420816257 ) ;
#11195 = FACE_OUTER_BOUND ( 'NONE', #7237, .T. ) ;
#11196 = FACE_OUTER_BOUND ( 'NONE', #7137, .T. ) ;
#11197 = ORIENTED_EDGE ( 'NONE', *, *, #13631, .F. ) ;
#11198 = CARTESIAN_POINT ( 'NONE',  ( 1.254255976358459757, 14.24071337840876694, -3.563435620217374478 ) ) ;
#11199 = CARTESIAN_POINT ( 'NONE',  ( 3.950837973638676281, 2.591948120962007884, -14.31366178983250670 ) ) ;
#11200 = CARTESIAN_POINT ( 'NONE',  ( 0.3137051932979792457, 8.442169467527008919, -10.83767969834794087 ) ) ;
#11201 = CARTESIAN_POINT ( 'NONE',  ( 0.4754618798421171855, 13.45049478164060019, 3.583352865732718495 ) ) ;
#11202 = CARTESIAN_POINT ( 'NONE',  ( -110.4113270445337918, -81.60345299795268659, -91.28051051278382033 ) ) ;
#11203 = VECTOR ( 'NONE', #14527, 1000.000000000000114 ) ;
#11204 = VECTOR ( 'NONE', #8287, 1000.000000000000114 ) ;
#11205 =( NAMED_UNIT ( * ) SI_UNIT ( $, .STERADIAN. ) SOLID_ANGLE_UNIT ( ) );
#11206 = EDGE_CURVE ( 'NONE', #7454, #13762, #10060, .T. ) ;
#11207 = AXIS2_PLACEMENT_3D ( 'NONE', #18345, #5250, #14044 ) ;
#11208 = DIRECTION ( 'NONE',  ( 0.7635533937278216055, 0.3620487483322444855, 0.5347026451755978460 ) ) ;
#11209 = CARTESIAN_POINT ( 'NONE',  ( 1.560000000000000053, 0.8660254037844389297, 1.500000000000000000 ) ) ;
#11211 = VERTEX_POINT ( 'NONE', #7907 ) ;
#11210 = DIRECTION ( 'NONE',  ( -0.000000000000000000, 0.000000000000000000, 1.000000000000000000 ) ) ;
#11212 = CARTESIAN_POINT ( 'NONE',  ( 2.320520222537280297, -10.64885284335050741, 11.60169517779339898 ) ) ;
#11213 = AXIS2_PLACEMENT_3D ( 'NONE', #9785, #2515, #17060 ) ;
#11214 = VERTEX_POINT ( 'NONE', #16405 ) ;
#11215 = EDGE_CURVE ( 'NONE', #2949, #7506, #10953, .T. ) ;
#11216 = B_SPLINE_CURVE_WITH_KNOTS ( 'NONE', 3,
 ( #12151, #13675, #18068, #15374, #3433, #18336, #9270 ),
 .UNSPECIFIED., .F., .F.,
 ( 4, 3, 4 ),
 ( 3.198396408832238080E-18, 0.0002299780670421061460, 0.0004597478348665241538 ),
 .UNSPECIFIED. ) ;
#11217 = CARTESIAN_POINT ( 'NONE',  ( 16.56753206892534891, 0.006669401563384923931, -0.006760771273036191367 ) ) ;
#11218 = CARTESIAN_POINT ( 'NONE',  ( 0.4862570985993252548, 10.79774104611373353, 8.769551628660776643 ) ) ;
#11219 = ORIENTED_EDGE ( 'NONE', *, *, #1340, .F. ) ;
#11220 = CARTESIAN_POINT ( 'NONE',  ( 8.522092701127531811, 6.946128462138595694, 0.3779863304871469154 ) ) ;
#11221 = VECTOR ( 'NONE', #10471, 1000.000000000000000 ) ;
#11222 = CARTESIAN_POINT ( 'NONE',  ( 3.950837973638668288, 0.000000000000000000, 0.000000000000000000 ) ) ;
#11223 = ORIENTED_EDGE ( 'NONE', *, *, #4614, .F. ) ;
#11224 = LINE ( 'NONE', #9763, #17825 ) ;
#11225 = COLOUR_RGB ( '', 0.72549020, 0.75294118, 0.79215686) ;
#11226 = CARTESIAN_POINT ( 'NONE',  ( 1.846138399168762101, 6.971848976711159551, -10.30487220521562541 ) ) ;
#11227 = LINE ( 'NONE', #15595, #7314 ) ;
#11228 = PLANE ( 'NONE',  #16646 ) ;
#11229 = CARTESIAN_POINT ( 'NONE',  ( 16.57605080000000086, 0.000000000000000000, 1.500000000000000000 ) ) ;
#11230 = APPLICATION_PROTOCOL_DEFINITION ( 'draft international standard', 'automotive_design', 1998, #16819 ) ;
#11231 = FACE_OUTER_BOUND ( 'NONE', #12134, .T. ) ;
#11232 = CARTESIAN_POINT ( 'NONE',  ( 1.846955891736120181, -4.094751675596620011, -11.74973605926568077 ) ) ;
#11233 = LINE ( 'NONE', #4047, #3488 ) ;
#11234 = CARTESIAN_POINT ( 'NONE',  ( 0.4754618798421162973, 13.45049478164060019, 3.583352865732715387 ) ) ;
#11235 = EDGE_CURVE ( 'NONE', #5038, #16664, #17932, .T. ) ;
#11236 = ADVANCED_FACE ( 'NONE', ( #7712 ), #13715, .F. ) ;
#11237 = CARTESIAN_POINT ( 'NONE',  ( 0.000000000000000000, 0.000000000000000000, 0.000000000000000000 ) ) ;
#11238 = CARTESIAN_POINT ( 'NONE',  ( 16.57210152137263393, -0.01214401161737629908, -0.008007331252333388036 ) ) ;
#11239 = ORIENTED_EDGE ( 'NONE', *, *, #16542, .F. ) ;
#11240 = ORIENTED_EDGE ( 'NONE', *, *, #2853, .T. ) ;
#11241 = ORIENTED_EDGE ( 'NONE', *, *, #1285, .F. ) ;
#11242 = VERTEX_POINT ( 'NONE', #14953 ) ;
#11243 = CIRCLE ( 'NONE', #14576, 16.06066017081991149 ) ;
#11244 = CARTESIAN_POINT ( 'NONE',  ( 1.847426409206471831, -0.06227732482761883653, -12.44303504652092229 ) ) ;
#11245 = CARTESIAN_POINT ( 'NONE',  ( 0.3720661004400037664, -10.73619472937695640, -8.694226082900707198 ) ) ;
#11246 = DIRECTION ( 'NONE',  ( 0.000000000000000000, 0.000000000000000000, 1.000000000000000000 ) ) ;
#11247 = DIRECTION ( 'NONE',  ( 0.000000000000000000, 0.000000000000000000, 1.000000000000000000 ) ) ;
#11248 = DIRECTION ( 'NONE',  ( 0.000000000000000000, 0.000000000000000000, 1.000000000000000000 ) ) ;
#11249 = FACE_OUTER_BOUND ( 'NONE', #3514, .T. ) ;
#11250 = CARTESIAN_POINT ( 'NONE',  ( 0.3151928479966097374, -6.943324943027912228E-05, -13.73922861026898623 ) ) ;
#11251 = CARTESIAN_POINT ( 'NONE',  ( 0.3150692679895942816, -13.11337225490255776, 4.099798979280796729 ) ) ;
#11252 = EDGE_CURVE ( 'NONE', #11465, #15522, #17585, .T. ) ;
#11253 = CARTESIAN_POINT ( 'NONE',  ( 2.747332970342022840, 7.289199830147106596, 14.63517873738950037 ) ) ;
#11254 = ADVANCED_FACE ( 'NONE', ( #12000 ), #4557, .F. ) ;
#11255 = EDGE_LOOP ( 'NONE', ( #13377, #12289, #6531, #9570 ) ) ;
#11256 = ADVANCED_FACE ( 'NONE', ( #631 ), #7756, .F. ) ;
#11257 = EDGE_CURVE ( 'NONE', #14985, #3963, #5717, .T. ) ;
#11258 = ORIENTED_EDGE ( 'NONE', *, *, #3555, .T. ) ;
#11259 = ORIENTED_EDGE ( 'NONE', *, *, #1048, .T. ) ;
#11260 = ORIENTED_EDGE ( 'NONE', *, *, #6533, .T. ) ;
#11261 =( BOUNDED_SURFACE ( )  B_SPLINE_SURFACE ( 3, 1, ( 
 ( #5987, #4849 ),
 ( #12014, #6382 ),
 ( #13534, #7532 ),
 ( #7433, #11823 ) ),
 .UNSPECIFIED., .F., .F., .T. ) 
 B_SPLINE_SURFACE_WITH_KNOTS ( ( 4, 4 ),
 ( 2, 2 ),
 ( 0.000000000000000000, 1.000000000000000000 ),
 ( 0.000000000000000000, 1.000000000000000000 ),
 .UNSPECIFIED. ) 
 GEOMETRIC_REPRESENTATION_ITEM ( )  RATIONAL_B_SPLINE_SURFACE ( (
 ( 1.000000000000000000, 1.000000000000000000),
 ( 0.9933953342250436691, 0.8357391271907733676),
 ( 0.9933953342250436691, 0.8357391271907733676),
 ( 1.000000000000000000, 1.000000000000000000) ) ) 
 REPRESENTATION_ITEM ( '' )  SURFACE ( )  );
#11262 = CARTESIAN_POINT ( 'NONE',  ( 3.950837973638668288, 0.000000000000000000, 0.000000000000000000 ) ) ;
#11263 = CARTESIAN_POINT ( 'NONE',  ( 1.321128355694181398E-14, -7.013167318348350499, 16.24521815286417237 ) ) ;
#11264 = CARTESIAN_POINT ( 'NONE',  ( 0.3720661004400040439, 4.951033743989640357, 12.89739157014194859 ) ) ;
#11265 = PLANE ( 'NONE',  #5069 ) ;
#11266 = CARTESIAN_POINT ( 'NONE',  ( 2.636624412714237309, 14.14563173255211126, 7.605649742762011556 ) ) ;
#11267 = ORIENTED_EDGE ( 'NONE', *, *, #9709, .F. ) ;
#11268 = DIRECTION ( 'NONE',  ( 0.000000000000000000, 0.000000000000000000, -1.000000000000000000 ) ) ;
#11269 = CARTESIAN_POINT ( 'NONE',  ( 1.977436885025426250, 7.806953934146316776, 13.27782258181756880 ) ) ;
#11270 = CARTESIAN_POINT ( 'NONE',  ( 6.273991221456205913, 3.109390318170344614, -12.00000000063437433 ) ) ;
#11271 = LINE ( 'NONE', #18516, #12723 ) ;
#11272 = B_SPLINE_CURVE_WITH_KNOTS ( 'NONE', 3,
 ( #8595, #12890, #1235, #16148, #8790, #4108 ),
 .UNSPECIFIED., .F., .F.,
 ( 4, 2, 4 ),
 ( 4.336808689942017736E-19, 0.001500839035891552006, 0.003001678071783103578 ),
 .UNSPECIFIED. ) ;
#11273 = CARTESIAN_POINT ( 'NONE',  ( 3.950837973638675393, -2.591948120961706792, -14.31366178983255466 ) ) ;
#11274 = CARTESIAN_POINT ( 'NONE',  ( 1.846138399168762101, -10.30487220521574976, 6.971848976710974810 ) ) ;
#11275 = DIRECTION ( 'NONE',  ( 0.000000000000000000, 0.000000000000000000, 1.000000000000000000 ) ) ;
#11276 = DIRECTION ( 'NONE',  ( -0.000000000000000000, -0.000000000000000000, 1.000000000000000000 ) ) ;
#11277 = VERTEX_POINT ( 'NONE', #17047 ) ;
#11279 = VERTEX_POINT ( 'NONE', #18382 ) ;
#11278 = CARTESIAN_POINT ( 'NONE',  ( 16.56822296793089322, 0.006547366384935510326, -0.007741272030791107074 ) ) ;
#11280 = CARTESIAN_POINT ( 'NONE',  ( 16.58200780006414732, -0.002844973367390960309, -0.01080144354108991157 ) ) ;
#11281 = EDGE_CURVE ( 'NONE', #2507, #996, #4682, .T. ) ;
#11282 = VECTOR ( 'NONE', #9806, 1000.000000000000114 ) ;
#11283 = CARTESIAN_POINT ( 'NONE',  ( 1.847412631396504246, -0.04315047898443813423, 12.44294644888238999 ) ) ;
#11284 = VECTOR ( 'NONE', #14242, 1000.000000000000114 ) ;
#11285 = VERTEX_POINT ( 'NONE', #13990 ) ;
#11286 = CARTESIAN_POINT ( 'NONE',  ( 3.074695600507223681, -13.70113613813211195, -7.366518011946086908 ) ) ;
#11287 = CARTESIAN_POINT ( 'NONE',  ( -5.926008024970758292, -7.500000000000000888, -16.97528233579634716 ) ) ;
#11288 = CARTESIAN_POINT ( 'NONE',  ( 2.750000000000000000, 0.000000000000000000, 0.000000000000000000 ) ) ;
#11289 = ORIENTED_EDGE ( 'NONE', *, *, #12790, .F. ) ;
#11290 = CARTESIAN_POINT ( 'NONE',  ( 0.4862570985993235340, 13.44146924561385958, -3.580942890621532371 ) ) ;
#11291 = CARTESIAN_POINT ( 'NONE',  ( 1.977228804422632713, -13.27756617201330336, -7.806978995470745808 ) ) ;
#11292 = CARTESIAN_POINT ( 'NONE',  ( 0.4385251269669950269, -13.84299131624728929, -0.7363879510386833749 ) ) ;
#11293 = CARTESIAN_POINT ( 'NONE',  ( 15.00000000000000711, -40.00000000000000000, 6.000000000000000000 ) ) ;
#11294 = DIRECTION ( 'NONE',  ( 1.000000000000000000, 0.000000000000000000, -0.000000000000000000 ) ) ;
#11295 = ADVANCED_FACE ( 'NONE', ( #12643 ), #2417, .T. ) ;
#11296 = FACE_OUTER_BOUND ( 'NONE', #3420, .T. ) ;
#11297 = EDGE_CURVE ( 'NONE', #9839, #5025, #714, .T. ) ;
#11298 = CARTESIAN_POINT ( 'NONE',  ( 0.3170788640506441158, 7.952793437297734691, -11.20690911610894958 ) ) ;
#11300 = ORIENTED_EDGE ( 'NONE', *, *, #2048, .T. ) ;
#11299 = CARTESIAN_POINT ( 'NONE',  ( 8.522092701127531811, -6.722964936702084948, -1.786985377232103600 ) ) ;
#11301 = CARTESIAN_POINT ( 'NONE',  ( 1.342453679581834924, -5.476372339889922003, -13.74702459364890039 ) ) ;
#11302 = EDGE_CURVE ( 'NONE', #978, #10313, #8175, .T. ) ;
#11303 = B_SPLINE_CURVE_WITH_KNOTS ( 'NONE', 3,
 ( #11701, #9030, #10663, #17829, #1768, #13227 ),
 .UNSPECIFIED., .F., .F.,
 ( 4, 2, 4 ),
 ( 2.710505431213761085E-19, 0.001657017934712013297, 0.003314035869424026594 ),
 .UNSPECIFIED. ) ;
#11304 = CARTESIAN_POINT ( 'NONE',  ( 0.4385251269669950269, -0.7363879510386354132, 13.84299131624729462 ) ) ;
#11305 = VERTEX_POINT ( 'NONE', #9690 ) ;
#11306 = FACE_OUTER_BOUND ( 'NONE', #4982, .T. ) ;
#11307 = CARTESIAN_POINT ( 'NONE',  ( 1.342453679581834924, 14.76648944001039254, -0.9602753779831244563 ) ) ;
#11308 = ORIENTED_EDGE ( 'NONE', *, *, #10895, .F. ) ;
#11309 = CARTESIAN_POINT ( 'NONE',  ( 0.3150686449036065317, -8.199336701264455129, -11.02450593298027570 ) ) ;
#11310 =( LENGTH_UNIT ( ) NAMED_UNIT ( * ) SI_UNIT ( .MILLI., .METRE. ) );
#11311 = LINE ( 'NONE', #11497, #2736 ) ;
#11312 = CARTESIAN_POINT ( 'NONE',  ( 1.918921323896324749, 7.860085869556325378, -9.738309537478915701 ) ) ;
#11313 = B_SPLINE_CURVE_WITH_KNOTS ( 'NONE', 3,
 ( #16588, #13962, #1047, #10564 ),
 .UNSPECIFIED., .F., .F.,
 ( 4, 4 ),
 ( 1.914591753770035818E-17, 0.002004993803842692549 ),
 .UNSPECIFIED. ) ;
#11314 = UNCERTAINTY_MEASURE_WITH_UNIT (LENGTH_MEASURE( 1.000000000000000082E-05 ), #10749, 'distance_accuracy_value', 'NONE');
#11315 = ADVANCED_FACE ( 'NONE', ( #5553 ), #17498, .F. ) ;
#11316 = ORIENTED_EDGE ( 'NONE', *, *, #9241, .F. ) ;
#11317 = PRESENTATION_STYLE_ASSIGNMENT (( #2330 ) ) ;
#11318 = CARTESIAN_POINT ( 'NONE',  ( 0.4862570985993235340, -13.44146924561378498, -3.580942890621813923 ) ) ;
#11319 = EDGE_CURVE ( 'NONE', #7003, #8226, #9590, .T. ) ;
#11320 = CARTESIAN_POINT ( 'NONE',  ( 0.3145729642390355241, -12.96842777670210189, 4.535980493005037140 ) ) ;
#11321 = CARTESIAN_POINT ( 'NONE',  ( 8.438534575730034959, -0.2320579683290609485, 6.862570336891074874 ) ) ;
#11322 = CARTESIAN_POINT ( 'NONE',  ( 2.636624412714236865, 0.000000000000000000, 0.000000000000000000 ) ) ;
#11323 = DIRECTION ( 'NONE',  ( 0.000000000000000000, 0.000000000000000000, 1.000000000000000000 ) ) ;
#11324 = VERTEX_POINT ( 'NONE', #9770 ) ;
#11325 = DIRECTION ( 'NONE',  ( 1.000000000000000000, 0.000000000000000000, -0.000000000000000000 ) ) ;
#11326 =( NAMED_UNIT ( * ) PLANE_ANGLE_UNIT ( ) SI_UNIT ( $, .RADIAN. ) );
#11327 = ORIENTED_EDGE ( 'NONE', *, *, #11252, .F. ) ;
#11328 = ORIENTED_EDGE ( 'NONE', *, *, #11830, .T. ) ;
#11329 = VERTEX_POINT ( 'NONE', #15602 ) ;
#11330 = CARTESIAN_POINT ( 'NONE',  ( 2.949999999999999734, 0.000000000000000000, 2.700000000000000178 ) ) ;
#11331 = ORIENTED_EDGE ( 'NONE', *, *, #8189, .F. ) ;
#11332 = CARTESIAN_POINT ( 'NONE',  ( 0.4384471787762835859, 13.39294437382618419, 3.577367180593594043 ) ) ;
#11333 = CARTESIAN_POINT ( 'NONE',  ( 16.56872352241294521, 0.01027347319884441834, -0.001821578298044677175 ) ) ;
#11334 = EDGE_CURVE ( 'NONE', #16657, #14151, #8353, .T. ) ;
#11335 = CARTESIAN_POINT ( 'NONE',  ( 0.3095370825347234511, 4.681152801286343923, -12.91933430393602933 ) ) ;
#11336 = CARTESIAN_POINT ( 'NONE',  ( 1.959212340397939123, 6.829000156128186561, 10.53510106265284563 ) ) ;
#11337 = DIRECTION ( 'NONE',  ( -1.000000000000000000, -0.000000000000000000, -0.000000000000000000 ) ) ;
#11338 = CONICAL_SURFACE ( 'NONE', #3693, 14.54644660717763927, 0.8559913436420816257 ) ;
#11339 = CARTESIAN_POINT ( 'NONE',  ( 0.3137051932979775248, -0.4596302728638797519, -13.73004976592202553 ) ) ;
#11340 = CARTESIAN_POINT ( 'NONE',  ( 2.747332970342022840, -11.45495994260709161, -11.66639548242820190 ) ) ;
#11341 = B_SPLINE_CURVE_WITH_KNOTS ( 'NONE', 3,
 ( #15860, #1330, #2940, #7172, #1528, #12985 ),
 .UNSPECIFIED., .F., .F.,
 ( 4, 2, 4 ),
 ( 3.556447555475521540E-17, 0.0001825746017570587236, 0.0003651492035140818855 ),
 .UNSPECIFIED. ) ;
#11342 = LINE ( 'NONE', #6951, #14543 ) ;
#11343 = ORIENTED_EDGE ( 'NONE', *, *, #6109, .T. ) ;
#11344 = ORIENTED_EDGE ( 'NONE', *, *, #12876, .F. ) ;
#11345 = ORIENTED_EDGE ( 'NONE', *, *, #10293, .T. ) ;
#11346 = ORIENTED_EDGE ( 'NONE', *, *, #3865, .T. ) ;
#11347 = FACE_OUTER_BOUND ( 'NONE', #18235, .T. ) ;
#11348 = CARTESIAN_POINT ( 'NONE',  ( 3.353306896162457029, 13.62210141459500079, -3.007732942432275181 ) ) ;
#11349 = CYLINDRICAL_SURFACE ( 'NONE', #10041, 5.000000000000004441 ) ;
#11350 = LINE ( 'NONE', #10094, #190 ) ;
#11351 = DIRECTION ( 'NONE',  ( 1.000000000000000000, 0.000000000000000000, 0.000000000000000000 ) ) ;
#11352 = ORIENTED_EDGE ( 'NONE', *, *, #17068, .F. ) ;
#11353 = DIRECTION ( 'NONE',  ( 0.000000000000000000, 0.000000000000000000, 1.000000000000000000 ) ) ;
#11354 = EDGE_CURVE ( 'NONE', #7378, #796, #1159, .T. ) ;
#11355 = ADVANCED_FACE ( 'NONE', ( #17133 ), #18653, .T. ) ;
#11356 = CARTESIAN_POINT ( 'NONE',  ( 2.123976203522053297, -1.531817366691861304, 15.54801196254786255 ) ) ;
#11357 = EDGE_CURVE ( 'NONE', #18215, #12560, #15963, .T. ) ;
#11358 = CARTESIAN_POINT ( 'NONE',  ( 8.522092701127531811, 2.505958102592713121, -6.489356537178164075 ) ) ;
#11359 = CARTESIAN_POINT ( 'NONE',  ( 0.3095370825347234511, 3.806662003783410242, 13.20347358821915940 ) ) ;
#11360 = CONICAL_SURFACE ( 'NONE', #17777, 14.54644660717763927, 0.8559913436420816257 ) ;
#11361 = CARTESIAN_POINT ( 'NONE',  ( 22.75000000000000000, 0.000000000000000000, 0.000000000000000000 ) ) ;
#11362 = DIRECTION ( 'NONE',  ( 1.000000000000000000, 0.000000000000000000, -0.000000000000000000 ) ) ;
#11363 = CARTESIAN_POINT ( 'NONE',  ( 0.3170788640506441158, -11.20690911610897800, -7.952793437297696499 ) ) ;
#11364 = CARTESIAN_POINT ( 'NONE',  ( 3.074695600507753479, -6.754521329825609932, -14.01296402267891317 ) ) ;
#11365 = VERTEX_POINT ( 'NONE', #15794 ) ;
#11367 = ORIENTED_EDGE ( 'NONE', *, *, #10048, .T. ) ;
#11366 = CARTESIAN_POINT ( 'NONE',  ( 1.342453679581834924, -9.456403821038714241, -11.38190519890864039 ) ) ;
#11368 = CARTESIAN_POINT ( 'NONE',  ( 0.3058872367615230181, 8.562166468153717958, 10.75034008168919009 ) ) ;
#11369 = EDGE_LOOP ( 'NONE', ( #16134, #1190, #8654, #5478 ) ) ;
#11370 = AXIS2_PLACEMENT_3D ( 'NONE', #14849, #14746, #13317 ) ;
#11371 = CARTESIAN_POINT ( 'NONE',  ( 16.56822296793089322, 0.01011126603341004106, 0.0007467251401288980180 ) ) ;
#11372 = ORIENTED_EDGE ( 'NONE', *, *, #11050, .F. ) ;
#11373 = CARTESIAN_POINT ( 'NONE',  ( 1.846138399168762101, 3.446241763653166590, -11.95493567637846866 ) ) ;
#11374 = CARTESIAN_POINT ( 'NONE',  ( -5.324905852942846352, -7.500000000000000888, -16.88120503408574180 ) ) ;
#11375 = DIRECTION ( 'NONE',  ( -1.000000000000000000, 0.000000000000000000, 0.000000000000000000 ) ) ;
#11376 = VERTEX_POINT ( 'NONE', #2686 ) ;
#11377 = FACE_OUTER_BOUND ( 'NONE', #16005, .T. ) ;
#11378 = CARTESIAN_POINT ( 'NONE',  ( 3.950837973638676281, -1.958075594453890789, 14.41405733518059940 ) ) ;
#11379 = CARTESIAN_POINT ( 'NONE',  ( 1.847372867223025628, 12.44269075185938789, 0.1054171785006922379 ) ) ;
#11380 = CARTESIAN_POINT ( 'NONE',  ( 3.074695600508242421, -2.093687500613561348, -15.41438262616270194 ) ) ;
#11381 = DIRECTION ( 'NONE',  ( 1.000000000000000000, 0.000000000000000000, 0.000000000000000000 ) ) ;
#11382 = ADVANCED_FACE ( 'NONE', ( #12464 ), #3196, .F. ) ;
#11383 = SHAPE_REPRESENTATION_RELATIONSHIP ( 'NONE' , 'NONE' ,  #18049, #556 ) ;
#11384 = DIRECTION ( 'NONE',  ( 0.000000000000000000, 0.000000000000000000, 1.000000000000000000 ) ) ;
#11385 = CARTESIAN_POINT ( 'NONE',  ( 16.56753206892534891, -0.008490833999798035742, 0.004253784598196731770 ) ) ;
#11387 = VERTEX_POINT ( 'NONE', #8623 ) ;
#11386 = DIRECTION ( 'NONE',  ( -0.000000000000000000, 0.000000000000000000, -1.000000000000000000 ) ) ;
#11388 = CARTESIAN_POINT ( 'NONE',  ( 1.562796894703937678, 0.000000000000000000, 1.500000000000000000 ) ) ;
#11389 = EDGE_CURVE ( 'NONE', #15773, #9839, #10516, .T. ) ;
#11390 = VECTOR ( 'NONE', #13138, 1000.000000000000000 ) ;
#11391 = CARTESIAN_POINT ( 'NONE',  ( 0.8740779401508862456, -13.31469722824359891, 5.211551231203810808 ) ) ;
#11392 = VERTEX_POINT ( 'NONE', #14546 ) ;
#11393 = CARTESIAN_POINT ( 'NONE',  ( 0.3145729642390374670, 3.952965287571295949, -13.15786090015079957 ) ) ;
#11394 = CARTESIAN_POINT ( 'NONE',  ( 0.4385251269669978580, 10.76637725024251857, 8.732456510146114681 ) ) ;
#11395 = VERTEX_POINT ( 'NONE', #1263 ) ;
#11396 = CARTESIAN_POINT ( 'NONE',  ( -61.35602477868047799, 9.999999999999973355, 3.000000000000002665 ) ) ;
#11397 = CARTESIAN_POINT ( 'NONE',  ( 0.3058872367615230181, -13.72992299905060598, 0.6080468242580479021 ) ) ;
#11398 = VECTOR ( 'NONE', #3070, 1000.000000000000000 ) ;
#11399 = DIRECTION ( 'NONE',  ( 1.000000000000000000, 0.000000000000000000, 0.000000000000000000 ) ) ;
#11400 = ADVANCED_FACE ( 'NONE', ( #4240 ), #12306, .T. ) ;
#11401 = CARTESIAN_POINT ( 'NONE',  ( 0.3151928479966097374, 0.000000000000000000, -13.73922861026898623 ) ) ;
#11402 = DIRECTION ( 'NONE',  ( 0.000000000000000000, 0.000000000000000000, 1.000000000000000000 ) ) ;
#11403 = CIRCLE ( 'NONE', #107, 10.00000000000000888 ) ;
#11404 = ORIENTED_EDGE ( 'NONE', *, *, #7230, .F. ) ;
#11405 = AXIS2_PLACEMENT_3D ( 'NONE', #11915, #5878, #7529 ) ;
#11406 = ADVANCED_FACE ( 'NONE', ( #13206 ), #7752, .T. ) ;
#11407 = EDGE_CURVE ( 'NONE', #8226, #11439, #13826, .T. ) ;
#11408 = SHAPE_REPRESENTATION_RELATIONSHIP ( 'NONE' , 'NONE' ,  #9604, #16761 ) ;
#11409 = CARTESIAN_POINT ( 'NONE',  ( 16.56753206892534891, 0.004368917149005337522, 0.008432171035096464387 ) ) ;
#11410 = CARTESIAN_POINT ( 'NONE',  ( 0.3137051932979809665, -13.20008686438108647, 3.805684345189735307 ) ) ;
#11411 = CARTESIAN_POINT ( 'NONE',  ( 1.847426409206450959, -2.029922383240494730E-11, 12.44303504652081038 ) ) ;
#11412 = CARTESIAN_POINT ( 'NONE',  ( 0.3170788640506441158, 11.02668139258453905, -8.200855617524412722 ) ) ;
#11413 = DIRECTION ( 'NONE',  ( 1.000000000000000000, 0.000000000000000000, 0.000000000000000000 ) ) ;
#11414 = EDGE_LOOP ( 'NONE', ( #7468, #4293, #2171, #8340 ) ) ;
#11415 = CARTESIAN_POINT ( 'NONE',  ( 0.3137051932979775248, 10.83767969834815581, -8.442169467526731808 ) ) ;
#11416 = ORIENTED_EDGE ( 'NONE', *, *, #18690, .T. ) ;
#11417 = EDGE_CURVE ( 'NONE', #3140, #18684, #1552, .T. ) ;
#11418 = ORIENTED_EDGE ( 'NONE', *, *, #10909, .F. ) ;
#11419 = VECTOR ( 'NONE', #17382, 1000.000000000000000 ) ;
#11420 = MECHANICAL_DESIGN_GEOMETRIC_PRESENTATION_REPRESENTATION (  '', ( #14462 ), #8622 ) ;
#11421 = ORIENTED_EDGE ( 'NONE', *, *, #16253, .T. ) ;
#11422 = CARTESIAN_POINT ( 'NONE',  ( 16.56782317627811096, 0.008141063682853480823, -0.005492611183758445634 ) ) ;
#11423 = ORIENTED_EDGE ( 'NONE', *, *, #6506, .F. ) ;
#11424 = CARTESIAN_POINT ( 'NONE',  ( 8.438534575730034959, -5.415535776177489602, -4.221456476902725186 ) ) ;
#11425 = DIRECTION ( 'NONE',  ( 0.000000000000000000, 0.000000000000000000, -1.000000000000000000 ) ) ;
#11426 = CARTESIAN_POINT ( 'NONE',  ( 0.3058872367615226295, -0.6080468242581913429, 13.72992299905059888 ) ) ;
#11427 = FACE_OUTER_BOUND ( 'NONE', #3813, .T. ) ;
#11428 = CARTESIAN_POINT ( 'NONE',  ( 0.3132635586635958425, -12.89236642382225462, 4.743936529203192087 ) ) ;
#11429 = AXIS2_PLACEMENT_3D ( 'NONE', #14644, #11977, #9109 ) ;
#11430 = FACE_OUTER_BOUND ( 'NONE', #15386, .T. ) ;
#11431 = DIRECTION ( 'NONE',  ( 0.000000000000000000, 0.000000000000000000, 1.000000000000000000 ) ) ;
#11432 = EDGE_CURVE ( 'NONE', #1936, #7722, #5569, .T. ) ;
#11433 = ORIENTED_EDGE ( 'NONE', *, *, #13834, .T. ) ;
#11434 = B_SPLINE_CURVE_WITH_KNOTS ( 'NONE', 3,
 ( #312, #17608, #7589, #117, #7773, #13395 ),
 .UNSPECIFIED., .F., .F.,
 ( 4, 2, 4 ),
 ( 0.000000000000000000, 0.0002017457492448075543, 0.0004034914984896151085 ),
 .UNSPECIFIED. ) ;
#11435 = ORIENTED_EDGE ( 'NONE', *, *, #2680, .F. ) ;
#11436 = ADVANCED_FACE ( 'NONE', ( #17418 ), #6524, .T. ) ;
#11437 = ORIENTED_EDGE ( 'NONE', *, *, #5261, .F. ) ;
#11438 = ORIENTED_EDGE ( 'NONE', *, *, #1098, .F. ) ;
#11439 = VERTEX_POINT ( 'NONE', #10345 ) ;
#11440 = DIRECTION ( 'NONE',  ( 0.000000000000000000, 0.000000000000000000, 1.000000000000000000 ) ) ;
#11441 = CARTESIAN_POINT ( 'NONE',  ( 16.56753206892534891, -0.008432171035096412345, -0.004368917149004214288 ) ) ;
#11442 = AXIS2_PLACEMENT_3D ( 'NONE', #17151, #11246, #2516 ) ;
#11443 = CARTESIAN_POINT ( 'NONE',  ( 0.3150686449036038672, 7.951193823202562072, -11.20479228691389118 ) ) ;
#11444 = ORIENTED_EDGE ( 'NONE', *, *, #15609, .T. ) ;
#11445 = CARTESIAN_POINT ( 'NONE',  ( 2.002547531651519996, -12.17374746633575988, -3.242439124566779185 ) ) ;
#11446 = CARTESIAN_POINT ( 'NONE',  ( 8.522092701127531811, -3.777034505568564349, 5.841710761610117153 ) ) ;
#11447 = CARTESIAN_POINT ( 'NONE',  ( 3.338474662712863417, 7.499999999999999112, -16.12819240262157194 ) ) ;
#11448 = CARTESIAN_POINT ( 'NONE',  ( 1.562796894703937678, 1.488975241814732168E-15, 12.15840553252917289 ) ) ;
#11449 = CARTESIAN_POINT ( 'NONE',  ( 25.00000000000000000, -2.500000000000000444, -12.00000000000000000 ) ) ;
#11450 = CARTESIAN_POINT ( 'NONE',  ( 1.918921323896323639, -10.48468902844557071, 6.832782632379341692 ) ) ;
#11451 = PLANE ( 'NONE',  #9497 ) ;
#11452 = LINE ( 'NONE', #14502, #6324 ) ;
#11453 = ORIENTED_EDGE ( 'NONE', *, *, #7881, .T. ) ;
#11454 = AXIS2_PLACEMENT_3D ( 'NONE', #13588, #2303, #15121 ) ;
#11455 = CIRCLE ( 'NONE', #10876, 14.54644660717763927 ) ;
#11456 = ORIENTED_EDGE ( 'NONE', *, *, #4966, .T. ) ;
#11457 = FACE_OUTER_BOUND ( 'NONE', #15136, .T. ) ;
#11458 = EDGE_CURVE ( 'NONE', #12775, #15569, #11864, .T. ) ;
#11459 = ADVANCED_FACE ( 'NONE', ( #11595 ), #7299, .T. ) ;
#11460 = ADVANCED_FACE ( 'NONE', ( #10152 ), #5840, .T. ) ;
#11461 = ORIENTED_EDGE ( 'NONE', *, *, #7041, .T. ) ;
#11462 = ORIENTED_EDGE ( 'NONE', *, *, #5498, .F. ) ;
#11463 = B_SPLINE_CURVE_WITH_KNOTS ( 'NONE', 3,
 ( #2613, #4061, #15808, #12659, #5665, #17244, #13037, #18670, #7122, #9979, #8551, #1002, #12941 ),
 .UNSPECIFIED., .F., .F.,
 ( 4, 3, 3, 3, 4 ),
 ( 3.035766082959412415E-18, 0.0002299780670421045197, 0.0004599561239687880061, 0.0006896788984287874130, 0.0009194956271626412558 ),
 .UNSPECIFIED. ) ;
#11464 = CARTESIAN_POINT ( 'NONE',  ( 0.4862570985993252548, 12.97920246947879441, 5.003653737315533867 ) ) ;
#11465 = VERTEX_POINT ( 'NONE', #5938 ) ;
#11466 = DIRECTION ( 'NONE',  ( -0.000000000000000000, -0.5000000000000004441, 0.8660254037844383745 ) ) ;
#11467 = CARTESIAN_POINT ( 'NONE',  ( 1.847247051441592403, -12.44188156437794035, -0.1676840720646602112 ) ) ;
#11468 = CARTESIAN_POINT ( 'NONE',  ( 16.57210152137263393, 0.0006600038696347836076, 0.01453130299868640209 ) ) ;
#11469 = LINE ( 'NONE', #14514, #5951 ) ;
#11470 = VERTEX_POINT ( 'NONE', #11877 ) ;
#11471 = CARTESIAN_POINT ( 'NONE',  ( 0.3170788640506441158, 13.11595226728158003, 4.100430649998006771 ) ) ;
#11472 = CARTESIAN_POINT ( 'NONE',  ( 2.002547531651521773, 9.778737580845699995, 7.942910686618207983 ) ) ;
#11473 = VECTOR ( 'NONE', #8323, 1000.000000000000000 ) ;
#11474 = CARTESIAN_POINT ( 'NONE',  ( 1.846138399168762101, 12.43476674860266584, 0.4167076046095977149 ) ) ;
#11475 = CARTESIAN_POINT ( 'NONE',  ( 1.104287921197080512E-14, -7.013167318348350499, 25.01316734529528674 ) ) ;
#11476 = CARTESIAN_POINT ( 'NONE',  ( 0.000000000000000000, 5.817072295949927426E-16, -4.750000000000000000 ) ) ;
#11477 = DIRECTION ( 'NONE',  ( 0.000000000000000000, -1.000000000000000000, 0.000000000000000000 ) ) ;
#11478 = CARTESIAN_POINT ( 'NONE',  ( 0.000000000000000000, 0.000000000000000000, 3.000000000000000000 ) ) ;
#11479 = CARTESIAN_POINT ( 'NONE',  ( 0.3095370825347224519, 3.806662003783598536, -13.20347358821910433 ) ) ;
#11480 = ADVANCED_FACE ( 'NONE', ( #14733 ), #18232, .F. ) ;
#11481 = CARTESIAN_POINT ( 'NONE',  ( 1.847461586945730261, 7.286856109515200686, -10.08650590720928619 ) ) ;
#11483 = ORIENTED_EDGE ( 'NONE', *, *, #6019, .T. ) ;
#11482 = CARTESIAN_POINT ( 'NONE',  ( 3.377929128793395908, -13.92579934231096495, 1.296196549818894539 ) ) ;
#11484 = CARTESIAN_POINT ( 'NONE',  ( 16.56753206892534891, -0.004368917149004301892, 0.008432171035096367243 ) ) ;
#11485 = AXIS2_PLACEMENT_3D ( 'NONE', #9901, #8658, #12772 ) ;
#11486 = CARTESIAN_POINT ( 'NONE',  ( 0.3308579732647026761, -0.5950689966505304795, 13.74211098745268522 ) ) ;
#11487 = COLOUR_RGB ( '', 0.09019608, 0.27058824, 0.51372549) ;
#11488 = EDGE_CURVE ( 'NONE', #10380, #9401, #10441, .T. ) ;
#11489 = ORIENTED_EDGE ( 'NONE', *, *, #7834, .T. ) ;
#11490 = CARTESIAN_POINT ( 'NONE',  ( 0.3058872367615226295, -4.821066432589418582, 12.87003593440626403 ) ) ;
#11491 = EDGE_CURVE ( 'NONE', #5922, #15858, #16871, .T. ) ;
#11492 = B_SPLINE_CURVE_WITH_KNOTS ( 'NONE', 3,
 ( #18079, #3446, #7674, #4603 ),
 .UNSPECIFIED., .F., .F.,
 ( 4, 4 ),
 ( 1.524041208624749586E-16, 0.002004993803842462265 ),
 .UNSPECIFIED. ) ;
#11493 = CARTESIAN_POINT ( 'NONE',  ( 1.959283090834856189, 12.53713130127477804, -0.6676170829052656686 ) ) ;
#11494 = ORIENTED_EDGE ( 'NONE', *, *, #10206, .T. ) ;
#11495 = LINE ( 'NONE', #114, #7866 ) ;
#11496 = CARTESIAN_POINT ( 'NONE',  ( 16.57778382496167424, 0.01092721432669108844, -0.01018821665058837478 ) ) ;
#11497 = CARTESIAN_POINT ( 'NONE',  ( 8.522092701127531811, 1.786985377232031436, 6.722964936702105376 ) ) ;
#11498 = CARTESIAN_POINT ( 'NONE',  ( 0.3151928476913618549, -11.11514699826556196, 8.075884471919712482 ) ) ;
#11499 = CARTESIAN_POINT ( 'NONE',  ( 16.56822296793089322, 0.007741272030791174728, -0.006547366384936662183 ) ) ;
#11500 = VERTEX_POINT ( 'NONE', #3261 ) ;
#11501 = VECTOR ( 'NONE', #9955, 1000.000000000000000 ) ;
#11502 = FILL_AREA_STYLE_COLOUR ( '', #14237 ) ;
#11503 = CARTESIAN_POINT ( 'NONE',  ( 0.3095370825347234511, 13.20347358821919848, -3.806662003783274795 ) ) ;
#11504 = CARTESIAN_POINT ( 'NONE',  ( 16.56872352241294521, 0.001821578298044641397, 0.01027347319884442528 ) ) ;
#11505 = CARTESIAN_POINT ( 'NONE',  ( 0.4384471787762838635, -10.76632603192792459, 8.732395932355645485 ) ) ;
#11506 = CARTESIAN_POINT ( 'NONE',  ( 16.57778382496167424, -0.007244066302947598825, 0.01306626476309386518 ) ) ;
#11507 = CARTESIAN_POINT ( 'NONE',  ( 16.56679352167444819, -0.004277682826583350043, -0.008252760440870175046 ) ) ;
#11508 = AXIS2_PLACEMENT_3D ( 'NONE', #17114, #15672, #11210 ) ;
#11509 = ORIENTED_EDGE ( 'NONE', *, *, #13726, .T. ) ;
#11510 = CARTESIAN_POINT ( 'NONE',  ( 2.002547531651519996, -6.845637710436264456, 10.57595306287289638 ) ) ;
#11511 = ORIENTED_EDGE ( 'NONE', *, *, #13631, .T. ) ;
#11512 = CIRCLE ( 'NONE', #17937, 2.499999999999995115 ) ;
#11513 = PRESENTATION_LAYER_ASSIGNMENT (  '', '', ( #8169 ) ) ;
#11514 = ORIENTED_EDGE ( 'NONE', *, *, #3045, .F. ) ;
#11515 = CARTESIAN_POINT ( 'NONE',  ( 2.636624412715384391, -11.60464335004044223, -11.10302021258006278 ) ) ;
#11516 = EDGE_CURVE ( 'NONE', #3683, #16167, #2498, .T. ) ;
#11517 = VERTEX_POINT ( 'NONE', #7594 ) ;
#11518 = DIRECTION ( 'NONE',  ( 0.000000000000000000, -1.000000000000000000, 0.000000000000000000 ) ) ;
#11519 = ORIENTED_EDGE ( 'NONE', *, *, #6631, .T. ) ;
#11520 = DIRECTION ( 'NONE',  ( 0.000000000000000000, 0.000000000000000000, 1.000000000000000000 ) ) ;
#11521 = FACE_OUTER_BOUND ( 'NONE', #13883, .T. ) ;
#11522 = CARTESIAN_POINT ( 'NONE',  ( 8.438534575730034959, -6.598402093327866424, -1.899950616255257740 ) ) ;
#11523 = CARTESIAN_POINT ( 'NONE',  ( 16.56872352241294521, 0.01033355228142401709, -0.001442253899401843694 ) ) ;
#11524 = CARTESIAN_POINT ( 'NONE',  ( -194.9999999999999716, -5.000000000000024869, 6.000000000000005329 ) ) ;
#11525 = CARTESIAN_POINT ( 'NONE',  ( 1.959283090834838426, 3.239245055717136168, -12.12982544407801555 ) ) ;
#11526 = EDGE_CURVE ( 'NONE', #4766, #16711, #7131, .T. ) ;
#11527 = CARTESIAN_POINT ( 'NONE',  ( 16.56753206892534891, -0.004253784598196240843, 0.008490833999798906573 ) ) ;
#11528 = CARTESIAN_POINT ( 'NONE',  ( 0.3720661004400037664, 12.89739157014192550, 4.951033743989683877 ) ) ;
#11529 = VERTEX_POINT ( 'NONE', #10931 ) ;
#11530 =( BOUNDED_SURFACE ( )  B_SPLINE_SURFACE ( 3, 1, ( 
 ( #14065, #9669 ),
 ( #6806, #9840 ),
 ( #970, #18452 ),
 ( #2575, #15495 ) ),
 .UNSPECIFIED., .F., .F., .T. ) 
 B_SPLINE_SURFACE_WITH_KNOTS ( ( 4, 4 ),
 ( 2, 2 ),
 ( 0.000000000000000000, 1.000000000000000000 ),
 ( 0.000000000000000000, 1.000000000000000000 ),
 .UNSPECIFIED. ) 
 GEOMETRIC_REPRESENTATION_ITEM ( )  RATIONAL_B_SPLINE_SURFACE ( (
 ( 1.000000000000000000, 1.000000000000000000),
 ( 0.9593108457356467333, 0.9995965569486454649),
 ( 0.9593108457356467333, 0.9995965569486454649),
 ( 1.000000000000000000, 1.000000000000000000) ) ) 
 REPRESENTATION_ITEM ( '' )  SURFACE ( )  );
#11531 = ORIENTED_EDGE ( 'NONE', *, *, #17675, .T. ) ;
#11532 = AXIS2_PLACEMENT_3D ( 'NONE', #2520, #7128, #14012 ) ;
#11533 = VERTEX_POINT ( 'NONE', #12258 ) ;
#11534 = ORIENTED_EDGE ( 'NONE', *, *, #2512, .T. ) ;
#11535 = VERTEX_POINT ( 'NONE', #18180 ) ;
#11536 = CARTESIAN_POINT ( 'NONE',  ( 1.847461586945732703, 3.813310247068605552, -11.84459954310606378 ) ) ;
#11537 = CARTESIAN_POINT ( 'NONE',  ( 0.4862570985993235340, -5.003653737315397976, -12.97920246947884770 ) ) ;
#11538 = DIRECTION ( 'NONE',  ( -0.000000000000000000, -0.000000000000000000, -1.000000000000000000 ) ) ;
#11539 = ORIENTED_EDGE ( 'NONE', *, *, #13131, .T. ) ;
#11540 = CARTESIAN_POINT ( 'NONE',  ( 1.977228804421669262, 6.152949558600965041, 14.12033626431027322 ) ) ;
#11541 = ADVANCED_FACE ( 'NONE', ( #16748 ), #9688, .F. ) ;
#11542 = LINE ( 'NONE', #15926, #7456 ) ;
#11543 = CARTESIAN_POINT ( 'NONE',  ( 5.250594443112312604, 4.638468187398189002, -11.99999999738841083 ) ) ;
#11544 = CARTESIAN_POINT ( 'NONE',  ( 16.56753206892534891, -0.006669401563384967299, 0.006760771273036151469 ) ) ;
#11545 = CARTESIAN_POINT ( 'NONE',  ( 0.3151930723728477157, -11.16020735774772277, 8.013866567350856229 ) ) ;
#11546 = AXIS2_PLACEMENT_3D ( 'NONE', #18850, #5742, #18748 ) ;
#11547 = CARTESIAN_POINT ( 'NONE',  ( 0.000000000000000000, 0.000000000000000000, 7.000000000000000000 ) ) ;
#11548 = DIRECTION ( 'NONE',  ( 0.000000000000000000, 0.000000000000000000, 1.000000000000000000 ) ) ;
#11549 = PLANE ( 'NONE',  #952 ) ;
#11550 = CARTESIAN_POINT ( 'NONE',  ( 1.847247051441598176, -4.004229874809106526, 11.78111530882021185 ) ) ;
#11551 = VERTEX_POINT ( 'NONE', #16375 ) ;
#11552 = EDGE_CURVE ( 'NONE', #570, #18779, #4903, .T. ) ;
#11553 = VERTEX_POINT ( 'NONE', #7971 ) ;
#11554 = VERTEX_POINT ( 'NONE', #7686 ) ;
#11555 = ORIENTED_EDGE ( 'NONE', *, *, #9778, .F. ) ;
#11556 = CARTESIAN_POINT ( 'NONE',  ( 3.950837973638676281, -12.81214529934979929, 6.888253895133251703 ) ) ;
#11557 = ORIENTED_EDGE ( 'NONE', *, *, #18545, .F. ) ;
#11558 = FACE_OUTER_BOUND ( 'NONE', #18070, .T. ) ;
#11559 = CARTESIAN_POINT ( 'NONE',  ( 1.847380140988740926, 11.86779270755359050, 3.740232970470796392 ) ) ;
#11560 = LINE ( 'NONE', #17283, #11419 ) ;
#11561 = CARTESIAN_POINT ( 'NONE',  ( 0.3095370825347224519, -3.806662003783324089, -13.20347358821918249 ) ) ;
#11562 = AXIS2_PLACEMENT_3D ( 'NONE', #12839, #13030, #10165 ) ;
#11563 = EDGE_LOOP ( 'NONE', ( #7042, #2980, #10846, #7932, #18051 ) ) ;
#11564 = DIRECTION ( 'NONE',  ( 0.000000000000000000, -0.000000000000000000, -1.000000000000000000 ) ) ;
#11565 = CARTESIAN_POINT ( 'NONE',  ( 0.3148208552358936485, -4.463611911212133521, -12.99355031785210102 ) ) ;
#11566 = DIRECTION ( 'NONE',  ( -1.000000000000000000, 0.000000000000000000, 0.000000000000000000 ) ) ;
#11567 =( BOUNDED_SURFACE ( )  B_SPLINE_SURFACE ( 3, 1, ( 
 ( #17175, #17467 ),
 ( #2820, #3994 ),
 ( #8305, #7151 ),
 ( #15640, #5694 ) ),
 .UNSPECIFIED., .F., .F., .T. ) 
 B_SPLINE_SURFACE_WITH_KNOTS ( ( 4, 4 ),
 ( 2, 2 ),
 ( 0.000000000000000000, 1.000000000000000000 ),
 ( 0.000000000000000000, 1.000000000000000000 ),
 .UNSPECIFIED. ) 
 GEOMETRIC_REPRESENTATION_ITEM ( )  RATIONAL_B_SPLINE_SURFACE ( (
 ( 1.000000000000000000, 1.000000000000000000),
 ( 0.7792777138730158093, 0.9689936506012928330),
 ( 0.7792777138730158093, 0.9689936506012928330),
 ( 1.000000000000000000, 1.000000000000000000) ) ) 
 REPRESENTATION_ITEM ( '' )  SURFACE ( )  );
#11568 = CARTESIAN_POINT ( 'NONE',  ( 0.3148208552358935930, -13.13564827777586785, -4.026279359288564841 ) ) ;
#11569 = EDGE_CURVE ( 'NONE', #11211, #1652, #15285, .T. ) ;
#11570 = CARTESIAN_POINT ( 'NONE',  ( 1.847412631396506022, 11.82061107079964124, 3.886120457021434493 ) ) ;
#11571 = EDGE_CURVE ( 'NONE', #5025, #678, #10964, .T. ) ;
#11572 = SURFACE_STYLE_USAGE ( .BOTH. , #5195 ) ;
#11573 = DIRECTION ( 'NONE',  ( 0.000000000000000000, 0.000000000000000000, -1.000000000000000000 ) ) ;
#11574 = LINE ( 'NONE', #17392, #5580 ) ;
#11575 = VERTEX_POINT ( 'NONE', #7883 ) ;
#11576 = CARTESIAN_POINT ( 'NONE',  ( 1.846613052777651198, 7.035606253495462425, -10.26230975746752350 ) ) ;
#11578 = ORIENTED_EDGE ( 'NONE', *, *, #9576, .F. ) ;
#11577 = CARTESIAN_POINT ( 'NONE',  ( 2.705023505549862595, -13.27418276223636795, 0.8488853074252508124 ) ) ;
#11579 = CARTESIAN_POINT ( 'NONE',  ( 8.522092701127531811, -4.388629235579537102, -5.397361180353192012 ) ) ;
#11580 = VERTEX_POINT ( 'NONE', #9392 ) ;
#11581 = CARTESIAN_POINT ( 'NONE',  ( 0.3137051932979792457, -13.20008686438103140, -3.805684345189927154 ) ) ;
#11582 = AXIS2_PLACEMENT_3D ( 'NONE', #8860, #13159, #6968 ) ;
#11583 = ORIENTED_EDGE ( 'NONE', *, *, #4126, .F. ) ;
#11584 = CARTESIAN_POINT ( 'NONE',  ( 1.847034903785825577, 9.929438108952146180, 7.498375632854650696 ) ) ;
#11585 = CARTESIAN_POINT ( 'NONE',  ( 2.864513242452144226, -7.500000000000000888, -15.84899838955148432 ) ) ;
#11586 = ORIENTED_EDGE ( 'NONE', *, *, #4292, .T. ) ;
#11587 = DIRECTION ( 'NONE',  ( 1.000000000000000000, 0.000000000000000000, 0.000000000000000000 ) ) ;
#11588 = DIRECTION ( 'NONE',  ( 0.000000000000000000, 0.000000000000000000, 1.000000000000000000 ) ) ;
#11589 = CARTESIAN_POINT ( 'NONE',  ( 2.949999999999999734, 0.000000000000000000, 0.000000000000000000 ) ) ;
#11590 = CARTESIAN_POINT ( 'NONE',  ( 1.136782529653004747, -45.00000000000000000, 3.000000000000000000 ) ) ;
#11591 = EDGE_CURVE ( 'NONE', #10186, #18408, #3457, .T. ) ;
#11592 = ORIENTED_EDGE ( 'NONE', *, *, #15896, .T. ) ;
#11593 = ADVANCED_FACE ( 'NONE', ( #13695 ), #1767, .F. ) ;
#11594 = EDGE_CURVE ( 'NONE', #16417, #5702, #9751, .T. ) ;
#11595 = FACE_OUTER_BOUND ( 'NONE', #367, .T. ) ;
#11596 = FACE_OUTER_BOUND ( 'NONE', #1013, .T. ) ;
#11597 = LINE ( 'NONE', #2871, #3706 ) ;
#11598 = CARTESIAN_POINT ( 'NONE',  ( 1.847168016377985333, 4.022276579849959788, 11.77471791462000184 ) ) ;
#11599 = FACE_OUTER_BOUND ( 'NONE', #2978, .T. ) ;
#11600 = ORIENTED_EDGE ( 'NONE', *, *, #5244, .T. ) ;
#11601 = DIRECTION ( 'NONE',  ( -0.7561779333270775005, 0.3559159372837393809, -0.5491072561318300904 ) ) ;
#11602 = ORIENTED_EDGE ( 'NONE', *, *, #4609, .T. ) ;
#11603 = ORIENTED_EDGE ( 'NONE', *, *, #8782, .F. ) ;
#11604 = CARTESIAN_POINT ( 'NONE',  ( 1.342453679581834924, -11.38190519890860131, 9.456403821038760427 ) ) ;
#11605 = VERTEX_POINT ( 'NONE', #14145 ) ;
#11606 = CARTESIAN_POINT ( 'NONE',  ( 3.950837973638668288, 0.000000000000000000, 0.000000000000000000 ) ) ;
#11607 = ORIENTED_EDGE ( 'NONE', *, *, #17295, .T. ) ;
#11608 = DIRECTION ( 'NONE',  ( -6.938893903907227392E-16, 0.000000000000000000, 1.000000000000000000 ) ) ;
#11609 = CARTESIAN_POINT ( 'NONE',  ( 0.3058872367615226295, -10.75034008168909416, -8.562166468153835197 ) ) ;
#11610 = CARTESIAN_POINT ( 'NONE',  ( 0.3142014840576498602, -8.382000553815529997, 10.88517824918540278 ) ) ;
#11611 = CARTESIAN_POINT ( 'NONE',  ( 16.56753206892534891, 0.004368917149005333185, 0.008432171035096464387 ) ) ;
#11612 = VECTOR ( 'NONE', #9584, 1000.000000000000000 ) ;
#11613 = SHAPE_REPRESENTATION_RELATIONSHIP ( 'NONE' , 'NONE' ,  #16816, #17679 ) ;
#11614 = CARTESIAN_POINT ( 'NONE',  ( 0.3308579732647013438, -3.680601586799781000, -13.25341063505879546 ) ) ;
#11615 = CARTESIAN_POINT ( 'NONE',  ( 0.3137051932979792457, -10.83767969834796929, -8.442169467526971616 ) ) ;
#11616 = VERTEX_POINT ( 'NONE', #8060 ) ;
#11617 = EDGE_CURVE ( 'NONE', #11535, #11022, #9836, .T. ) ;
#11618 = DIRECTION ( 'NONE',  ( -1.000000000000000000, -0.000000000000000000, -0.000000000000000000 ) ) ;
#11619 = DIRECTION ( 'NONE',  ( -0.000000000000000000, -0.000000000000000000, 1.000000000000000000 ) ) ;
#11620 = VERTEX_POINT ( 'NONE', #9664 ) ;
#11621 = ORIENTED_EDGE ( 'NONE', *, *, #9822, .F. ) ;
#11622 = EDGE_CURVE ( 'NONE', #4533, #14938, #2568, .T. ) ;
#11623 = VERTEX_POINT ( 'NONE', #13964 ) ;
#11624 = ORIENTED_EDGE ( 'NONE', *, *, #1070, .F. ) ;
#11625 = VERTEX_POINT ( 'NONE', #3928 ) ;
#11626 = FACE_OUTER_BOUND ( 'NONE', #8451, .T. ) ;
#11627 = CARTESIAN_POINT ( 'NONE',  ( 0.3095370825347224519, 7.700448427571875420, 11.38092634279631099 ) ) ;
#11628 = CARTESIAN_POINT ( 'NONE',  ( 0.4754618798421162973, 10.80499583390512974, 8.775436892861156579 ) ) ;
#11629 = ORIENTED_EDGE ( 'NONE', *, *, #11281, .F. ) ;
#11630 = CARTESIAN_POINT ( 'NONE',  ( 2.002547531651519996, -0.6781519942172617998, 12.57989064830759318 ) ) ;
#11631 = DIRECTION ( 'NONE',  ( -0.000000000000000000, -1.000000000000000000, -0.000000000000000000 ) ) ;
#11632 = CONICAL_SURFACE ( 'NONE', #32, 14.54644660717763927, 0.8559913436420816257 ) ;
#11633 = LINE ( 'NONE', #7537, #13415 ) ;
#11634 = PRODUCT_DEFINITION ( 'UNKNOWN', '', #12039, #1 ) ;
#11635 = CARTESIAN_POINT ( 'NONE',  ( 1.321128355694181398E-14, -9.013167318348349610, 25.01316734529530095 ) ) ;
#11636 = CARTESIAN_POINT ( 'NONE',  ( 0.3150686449036064207, -11.02450593298024195, 8.199336701264503091 ) ) ;
#11637 = EDGE_CURVE ( 'NONE', #18802, #17659, #4793, .T. ) ;
#11638 = FACE_OUTER_BOUND ( 'NONE', #8396, .T. ) ;
#11639 = CARTESIAN_POINT ( 'NONE',  ( 0.4754618798421162973, -11.68486377711960955, -7.564402563418597403 ) ) ;
#11640 = EDGE_CURVE ( 'NONE', #17865, #1087, #18416, .T. ) ;
#11641 = CARTESIAN_POINT ( 'NONE',  ( 0.3132642857406524595, -12.89240536501342760, -4.743831191224519905 ) ) ;
#11642 =( BOUNDED_SURFACE ( )  B_SPLINE_SURFACE ( 3, 1, ( 
 ( #17666, #4660 ),
 ( #10390, #16224 ),
 ( #3107, #14779 ),
 ( #266, #17759 ) ),
 .UNSPECIFIED., .F., .F., .T. ) 
 B_SPLINE_SURFACE_WITH_KNOTS ( ( 4, 4 ),
 ( 2, 2 ),
 ( 0.000000000000000000, 1.000000000000000000 ),
 ( 0.000000000000000000, 1.000000000000000000 ),
 .UNSPECIFIED. ) 
 GEOMETRIC_REPRESENTATION_ITEM ( )  RATIONAL_B_SPLINE_SURFACE ( (
 ( 1.000000000000000000, 1.000000000000000000),
 ( 0.9933953342250438912, 0.8357391271907739227),
 ( 0.9933953342250438912, 0.8357391271907739227),
 ( 1.000000000000000000, 1.000000000000000000) ) ) 
 REPRESENTATION_ITEM ( '' )  SURFACE ( )  );
#11643 = CARTESIAN_POINT ( 'NONE',  ( 0.3137051932979792457, -7.698472063774386420, -11.37800749014139612 ) ) ;
#11644 = ORIENTED_EDGE ( 'NONE', *, *, #17326, .F. ) ;
#11645 = ORIENTED_EDGE ( 'NONE', *, *, #1825, .T. ) ;
#11646 = EDGE_LOOP ( 'NONE', ( #7721, #11418, #12672, #8532 ) ) ;
#11647 = AXIS2_PLACEMENT_3D ( 'NONE', #609, #12260, #18090 ) ;
#11648 = ORIENTED_EDGE ( 'NONE', *, *, #1729, .T. ) ;
#11649 = CARTESIAN_POINT ( 'NONE',  ( 4.755015822784811164, -4.336808689942017736E-16, 0.000000000000000000 ) ) ;
#11650 = ADVANCED_FACE ( 'NONE', ( #11296 ), #690, .F. ) ;
#11651 = VERTEX_POINT ( 'NONE', #15398 ) ;
#11652 = CARTESIAN_POINT ( 'NONE',  ( 1.918918678667043576, 3.258447776120001915, -12.08296592096904298 ) ) ;
#11653 = CARTESIAN_POINT ( 'NONE',  ( 3.664313757352970047, -9.645155442698829518, 10.50730552161229880 ) ) ;
#11654 = LINE ( 'NONE', #5807, #1338 ) ;
#11655 = CARTESIAN_POINT ( 'NONE',  ( 16.56679352167444819, 0.004277682826583292797, 0.008252760440870202802 ) ) ;
#11656 = ORIENTED_EDGE ( 'NONE', *, *, #17240, .F. ) ;
#11657 = DIRECTION ( 'NONE',  ( -5.782411586589358625E-16, 1.000000000000000000, 0.000000000000000000 ) ) ;
#11658 = CARTESIAN_POINT ( 'NONE',  ( 0.3137051932979757485, -4.679953077377398074, -12.91601973349275134 ) ) ;
#11659 = CARTESIAN_POINT ( 'NONE',  ( 2.747332970342022840, -7.555624153089749662, 14.49942876448589679 ) ) ;
#11660 = DIRECTION ( 'NONE',  ( -1.000000000000000000, -0.000000000000000000, -0.000000000000000000 ) ) ;
#11661 = CARTESIAN_POINT ( 'NONE',  ( 0.3132642857406529591, -8.495623922778147374, 10.79548167658031588 ) ) ;
#11662 = CARTESIAN_POINT ( 'NONE',  ( 1.959283090834840646, -6.829027319138321062, 10.53516775895158020 ) ) ;
#11663 = DIRECTION ( 'NONE',  ( 0.000000000000000000, 0.000000000000000000, 1.000000000000000000 ) ) ;
#11664 = ORIENTED_EDGE ( 'NONE', *, *, #109, .F. ) ;
#11665 = AXIS2_PLACEMENT_3D ( 'NONE', #1419, #7163, #12975 ) ;
#11666 = CARTESIAN_POINT ( 'NONE',  ( 2.636624412717099908, 11.60464335004051861, -11.10302021258208249 ) ) ;
#11668 = ORIENTED_EDGE ( 'NONE', *, *, #8176, .T. ) ;
#11667 = CARTESIAN_POINT ( 'NONE',  ( 0.3148208552358962575, 0.2299193288887468323, 13.73693263646118190 ) ) ;
#11669 = CARTESIAN_POINT ( 'NONE',  ( 3.943463214271659518E-15, -27.00000000000000000, 22.91316734529526045 ) ) ;
#11670 = EDGE_CURVE ( 'NONE', #8373, #13548, #10022, .T. ) ;
#11671 = ORIENTED_EDGE ( 'NONE', *, *, #2206, .T. ) ;
#11672 = CARTESIAN_POINT ( 'NONE',  ( 2.636624412715138366, -15.91454522070249311, -2.161493821597819665 ) ) ;
#11673 = CARTESIAN_POINT ( 'NONE',  ( 5.288115175735552675, -4.595214139558242650, -11.99999999743901746 ) ) ;
#11674 = SHAPE_REPRESENTATION ( 'Ergonomic Rotary Turning Knob', ( #2030 ), #9034 ) ;
#11675 = ORIENTED_EDGE ( 'NONE', *, *, #15265, .F. ) ;
#11676 = LINE ( 'NONE', #1254, #5106 ) ;
#11677 = DIRECTION ( 'NONE',  ( -0.8571673007021134438, 1.049727191138620051E-16, 0.5150380749100522682 ) ) ;
#11678 = CARTESIAN_POINT ( 'NONE',  ( 1.847372867223022297, -10.00438561114518521, -7.398914411685100667 ) ) ;
#11679 = FACE_OUTER_BOUND ( 'NONE', #8917, .T. ) ;
#11680 = AXIS2_PLACEMENT_3D ( 'NONE', #14379, #6760, #5406 ) ;
#11681 = CARTESIAN_POINT ( 'NONE',  ( 16.56753206892534891, 0.008490833999798920451, 0.004253784598196212220 ) ) ;
#11682 = CARTESIAN_POINT ( 'NONE',  ( 2.747332970342022840, -16.12459247543624130, -2.705255688518015234 ) ) ;
#11683 = CARTESIAN_POINT ( 'NONE',  ( 2.636624412716902288, 7.605649742760546950, -14.14563173255513995 ) ) ;
#11684 = FACE_BOUND ( 'NONE', #4890, .T. ) ;
#11685 = ORIENTED_EDGE ( 'NONE', *, *, #4371, .T. ) ;
#11686 = CARTESIAN_POINT ( 'NONE',  ( 0.000000000000000000, 0.000000000000000000, -12.00000000000000000 ) ) ;
#11687 = CARTESIAN_POINT ( 'NONE',  ( 16.56753206892534891, 0.009389754735541551434, -0.001421777558676823056 ) ) ;
#11688 = VERTEX_POINT ( 'NONE', #5533 ) ;
#11689 = EDGE_CURVE ( 'NONE', #1651, #3145, #2216, .T. ) ;
#11690 = EDGE_CURVE ( 'NONE', #4766, #8069, #8954, .T. ) ;
#11691 = ADVANCED_FACE ( 'NONE', ( #5175 ), #8417, .F. ) ;
#11692 = ORIENTED_EDGE ( 'NONE', *, *, #3211, .T. ) ;
#11693 = DIRECTION ( 'NONE',  ( -1.000000000000000000, 0.000000000000000000, 0.000000000000000000 ) ) ;
#11694 = VERTEX_POINT ( 'NONE', #17203 ) ;
#11695 = FACE_OUTER_BOUND ( 'NONE', #8234, .T. ) ;
#11696 = ORIENTED_EDGE ( 'NONE', *, *, #11755, .T. ) ;
#11697 = AXIS2_PLACEMENT_3D ( 'NONE', #14428, #4394, #5915 ) ;
#11698 = CARTESIAN_POINT ( 'NONE',  ( 0.3307726912345211323, -0.5948952607471654774, -13.74203354050372461 ) ) ;
#11699 = CARTESIAN_POINT ( 'NONE',  ( 16.56872352241294521, 0.001821578298043785094, -0.01027347319884367241 ) ) ;
#11700 = FACE_OUTER_BOUND ( 'NONE', #14229, .T. ) ;
#11701 = CARTESIAN_POINT ( 'NONE',  ( 0.4862570985993235340, 7.559321496869593204, -11.67702470553357053 ) ) ;
#11702 = UNCERTAINTY_MEASURE_WITH_UNIT (LENGTH_MEASURE( 1.000000000000000082E-05 ), #6049, 'distance_accuracy_value', 'NONE');
#11703 = CARTESIAN_POINT ( 'NONE',  ( 0.3150692679895986670, -8.199139630396084399, 11.02465386701225469 ) ) ;
#11704 = DIRECTION ( 'NONE',  ( 0.000000000000000000, -1.000000000000000000, 0.000000000000000000 ) ) ;
#11705 = EDGE_CURVE ( 'NONE', #1072, #13213, #6623, .T. ) ;
#11706 = B_SPLINE_CURVE_WITH_KNOTS ( 'NONE', 3,
 ( #9506, #7714, #4839, #18024, #1969, #10668, #438, #6458, #12282, #15331, #4928, #12099, #10763 ),
 .UNSPECIFIED., .F., .F.,
 ( 4, 3, 3, 3, 4 ),
 ( 3.127317220692750759E-18, 0.0002299780670421087210, 0.0004599561239687931019, 0.0006896788984287912077, 0.0009194956271626412558 ),
 .UNSPECIFIED. ) ;
#11707 = SURFACE_SIDE_STYLE ('',( #4350 ) ) ;
#11708 = CARTESIAN_POINT ( 'NONE',  ( 1.847168016377985778, 0.1868244120189564983, 12.44137401948661115 ) ) ;
#11709 = CARTESIAN_POINT ( 'NONE',  ( 1.136782529653004747, -45.00000000000000000, 6.000000000000000000 ) ) ;
#11710 = CARTESIAN_POINT ( 'NONE',  ( 1.342453679581834924, 12.51077660954466353, 7.902645620902494450 ) ) ;
#11711 = CARTESIAN_POINT ( 'NONE',  ( 2.705023505549866591, -8.489131503859701056, -10.24007717649589821 ) ) ;
#11712 = VECTOR ( 'NONE', #4242, 1000.000000000000114 ) ;
#11713 = ORIENTED_EDGE ( 'NONE', *, *, #6196, .F. ) ;
#11714 = CIRCLE ( 'NONE', #8363, 4.999999999999997335 ) ;
#11715 = DIRECTION ( 'NONE',  ( -1.000000000000000000, 0.000000000000000000, 0.000000000000000000 ) ) ;
#11716 = VERTEX_POINT ( 'NONE', #5265 ) ;
#11717 = ORIENTED_EDGE ( 'NONE', *, *, #15596, .F. ) ;
#11718 = EDGE_LOOP ( 'NONE', ( #16435, #16188, #11887, #15294 ) ) ;
#11719 = VERTEX_POINT ( 'NONE', #11110 ) ;
#11720 = CARTESIAN_POINT ( 'NONE',  ( 1.959212340397940899, -12.12975361829678178, 3.239239832448982170 ) ) ;
#11721 = B_SPLINE_CURVE_WITH_KNOTS ( 'NONE', 3,
 ( #1649, #1950, #7694, #11884, #3166, #3267, #13407, #4818, #323, #10649, #6152, #11980, #17815 ),
 .UNSPECIFIED., .F., .F.,
 ( 4, 3, 3, 3, 4 ),
 ( 1.734723475976807094E-18, 0.0002299780670421052245, 0.0004599561239687887651, 0.0006896788984287890393, 0.0009194956271626402800 ),
 .UNSPECIFIED. ) ;
#11722 = EDGE_CURVE ( 'NONE', #18645, #18680, #9938, .T. ) ;
#11723 = CARTESIAN_POINT ( 'NONE',  ( 20.00000000000000000, -2.500000000000000444, -16.99999999999999645 ) ) ;
#11724 = CARTESIAN_POINT ( 'NONE',  ( 0.8740764193764966050, 11.05257066464512405, 9.070946295053792241 ) ) ;
#11725 = ORIENTED_EDGE ( 'NONE', *, *, #17877, .F. ) ;
#11726 = DIRECTION ( 'NONE',  ( 0.7635533937278214944, -0.1790966170213922626, -0.6204116510013485408 ) ) ;
#11727 = CARTESIAN_POINT ( 'NONE',  ( 0.4862570985993235340, 0.7479633556562450547, 13.89016912371017831 ) ) ;
#11728 = AXIS2_PLACEMENT_3D ( 'NONE', #8787, #17479, #90 ) ;
#11729 = CARTESIAN_POINT ( 'NONE',  ( 1.254255976357838698, 9.426444230097315469, -11.25336128106935973 ) ) ;
#11730 = CARTESIAN_POINT ( 'NONE',  ( 3.377929128793396796, -1.296196549818846355, -13.92579934231097560 ) ) ;
#11731 = CARTESIAN_POINT ( 'NONE',  ( 1.977228804422197062, -15.04020501276157518, -3.321884655131998265 ) ) ;
#11732 = EDGE_CURVE ( 'NONE', #8583, #15844, #11574, .T. ) ;
#11733 = CARTESIAN_POINT ( 'NONE',  ( 1.847461586945734702, 11.82388984758123840, -3.877048136045254001 ) ) ;
#11734 = CARTESIAN_POINT ( 'NONE',  ( 2.636624412714236865, 0.000000000000000000, 0.000000000000000000 ) ) ;
#11735 = B_SPLINE_CURVE_WITH_KNOTS ( 'NONE', 3,
 ( #6188, #7539, #15070, #459 ),
 .UNSPECIFIED., .F., .F.,
 ( 4, 4 ),
 ( 2.006682199098010609E-17, 0.003005512676784846595 ),
 .UNSPECIFIED. ) ;
#11736 = CARTESIAN_POINT ( 'NONE',  ( 0.3142011359265350912, -11.33549115679417696, -7.762194356530893735 ) ) ;
#11737 = B_SPLINE_CURVE_WITH_KNOTS ( 'NONE', 3,
 ( #3895, #15544, #7842, #8656, #12860, #11536, #1014, #7048, #15920, #17455, #4362, #10187, #7138 ),
 .UNSPECIFIED., .F., .F.,
 ( 4, 3, 3, 3, 4 ),
 ( 1.734723475976806902E-18, 0.0002299804304191479859, 0.0004599608082120235455, 0.0006467586077647999570, 0.0008336169836825983986 ),
 .UNSPECIFIED. ) ;
#11738 = CARTESIAN_POINT ( 'NONE',  ( 1.846138399168762101, 6.971848976711011225, 10.30487220521572667 ) ) ;
#11739 = ORIENTED_EDGE ( 'NONE', *, *, #13914, .F. ) ;
#11740 = ORIENTED_EDGE ( 'NONE', *, *, #4238, .T. ) ;
#11741 = VECTOR ( 'NONE', #1888, 1000.000000000000000 ) ;
#11742 = EDGE_LOOP ( 'NONE', ( #15451, #12329, #5978, #303 ) ) ;
#11743 = ORIENTED_EDGE ( 'NONE', *, *, #13287, .F. ) ;
#11744 = CARTESIAN_POINT ( 'NONE',  ( 2.636624412717099908, 14.46769361191384817, -6.973567714910368309 ) ) ;
#11745 = AXIS2_PLACEMENT_3D ( 'NONE', #9494, #12184, #11031 ) ;
#11746 = ORIENTED_EDGE ( 'NONE', *, *, #18071, .T. ) ;
#11747 = CARTESIAN_POINT ( 'NONE',  ( 2.636624412716045196, 11.10302021257998994, -11.60464335004042447 ) ) ;
#11748 = CARTESIAN_POINT ( 'NONE',  ( 16.56753206892534891, 0.006669401563385194548, 0.006760771273035138390 ) ) ;
#11749 = LINE ( 'NONE', #9257, #15088 ) ;
#11750 = CARTESIAN_POINT ( 'NONE',  ( 16.57778382496167424, 0.01018821665058833661, 0.01092721432669112661 ) ) ;
#11751 = ORIENTED_EDGE ( 'NONE', *, *, #462, .F. ) ;
#11752 = CARTESIAN_POINT ( 'NONE',  ( -194.9999999999999716, 4.999999999999973355, 6.000000000000000000 ) ) ;
#11753 = CARTESIAN_POINT ( 'NONE',  ( 2.002547531651519996, 3.242439124566649511, 12.17374746633579541 ) ) ;
#11754 = CARTESIAN_POINT ( 'NONE',  ( -6.500132120881464637, 2.599948583552246451, -12.00000000000000000 ) ) ;
#11755 = EDGE_CURVE ( 'NONE', #13344, #4154, #1627, .T. ) ;
#11756 =( BOUNDED_SURFACE ( )  B_SPLINE_SURFACE ( 3, 1, ( 
 ( #17797, #7380 ),
 ( #6037, #10526 ),
 ( #10627, #12058 ),
 ( #2955, #14819 ) ),
 .UNSPECIFIED., .F., .F., .T. ) 
 B_SPLINE_SURFACE_WITH_KNOTS ( ( 4, 4 ),
 ( 2, 2 ),
 ( 0.000000000000000000, 1.000000000000000000 ),
 ( 0.000000000000000000, 1.000000000000000000 ),
 .UNSPECIFIED. ) 
 GEOMETRIC_REPRESENTATION_ITEM ( )  RATIONAL_B_SPLINE_SURFACE ( (
 ( 1.000000000000000000, 1.000000000000000000),
 ( 0.9933953342250438912, 0.8357391271907739227),
 ( 0.9933953342250438912, 0.8357391271907739227),
 ( 1.000000000000000000, 1.000000000000000000) ) ) 
 REPRESENTATION_ITEM ( '' )  SURFACE ( )  );
#11757 = CARTESIAN_POINT ( 'NONE',  ( 0.3132642857406526260, 8.495623922778223758, -10.79548167658025193 ) ) ;
#11758 = CARTESIAN_POINT ( 'NONE',  ( 2.002547531651519996, -6.845637710436264456, 10.57595306287289638 ) ) ;
#11759 = AXIS2_PLACEMENT_3D ( 'NONE', #7729, #13538, #7827 ) ;
#11760 = CONICAL_SURFACE ( 'NONE', #3519, 12.15840553252917289, 0.7853981625000049371 ) ;
#11761 = ADVANCED_FACE ( 'NONE', ( #5722 ), #6518, .F. ) ;
#11762 = DIRECTION ( 'NONE',  ( 0.000000000000000000, 0.000000000000000000, 1.000000000000000000 ) ) ;
#11763 = ORIENTED_EDGE ( 'NONE', *, *, #16473, .T. ) ;
#11764 = CARTESIAN_POINT ( 'NONE',  ( 1.846955891736117072, 7.098901504650503291, -10.21904526726839002 ) ) ;
#11766 = ORIENTED_EDGE ( 'NONE', *, *, #3647, .F. ) ;
#11765 = CARTESIAN_POINT ( 'NONE',  ( 0.3142011359265339254, 0.3830873813806325301, 13.73310835363014171 ) ) ;
#11767 = CARTESIAN_POINT ( 'NONE',  ( 0.3148208552358927603, 7.888357771040864996, -11.24855514421867042 ) ) ;
#11768 = CARTESIAN_POINT ( 'NONE',  ( 0.000000000000000000, 0.000000000000000000, 0.000000000000000000 ) ) ;
#11769 = ORIENTED_EDGE ( 'NONE', *, *, #16443, .T. ) ;
#11770 = CARTESIAN_POINT ( 'NONE',  ( 0.3148213771069373057, 4.463459503829174224, -12.99360322443197724 ) ) ;
#11771 = B_SPLINE_CURVE_WITH_KNOTS ( 'NONE', 3,
 ( #9543, #8127, #16812, #12417, #760, #15462 ),
 .UNSPECIFIED., .F., .F.,
 ( 4, 2, 4 ),
 ( 0.000000000000000000, 0.001656992708823638600, 0.003313985417647277200 ),
 .UNSPECIFIED. ) ;
#11772 = PRESENTATION_LAYER_ASSIGNMENT (  '', '', ( #12079 ) ) ;
#11773 = CARTESIAN_POINT ( 'NONE',  ( 6.454593536054717973, -2.712332671582271093, -12.00000000018537882 ) ) ;
#11774 = TOROIDAL_SURFACE ( 'NONE', #4443, 5.000000000000005329, 5.000000000000000000 ) ;
#11775 = VERTEX_POINT ( 'NONE', #15867 ) ;
#11776 = CARTESIAN_POINT ( 'NONE',  ( -997.5739745962155212, 0.000000000000000000, 0.000000000000000000 ) ) ;
#11777 = CARTESIAN_POINT ( 'NONE',  ( 2.123976203522053297, -7.899625852120107261, -13.47898556379321633 ) ) ;
#11778 = CARTESIAN_POINT ( 'NONE',  ( 16.57605080000000086, 0.000000000000000000, 2.500000000000000000 ) ) ;
#11779 = CARTESIAN_POINT ( 'NONE',  ( 16.56872352241294521, -0.009207754980063714498, -0.004907101719994726684 ) ) ;
#11780 = ADVANCED_FACE ( 'NONE', ( #1336 ), #8604, .T. ) ;
#11781 = CARTESIAN_POINT ( 'NONE',  ( 3.950837973638668288, 0.000000000000000000, 0.000000000000000000 ) ) ;
#11782 = EDGE_CURVE ( 'NONE', #5854, #16571, #9262, .T. ) ;
#11783 = CYLINDRICAL_SURFACE ( 'NONE', #11546, 5.000000000000000000 ) ;
#11784 = VECTOR ( 'NONE', #5214, 999.9999999999998863 ) ;
#11785 = CARTESIAN_POINT ( 'NONE',  ( 1.959283090834855745, 0.6676170829052219258, 12.53713130127477982 ) ) ;
#11786 = CARTESIAN_POINT ( 'NONE',  ( 3.950837973638675393, 6.888253895133292559, 12.81214529934977797 ) ) ;
#11787 = CARTESIAN_POINT ( 'NONE',  ( 16.58200780006414732, 0.008650561019685807859, 0.007066318000006031885 ) ) ;
#11788 = CIRCLE ( 'NONE', #2033, 5.000000000000000888 ) ;
#11789 = ORIENTED_EDGE ( 'NONE', *, *, #15319, .F. ) ;
#11790 = CARTESIAN_POINT ( 'NONE',  ( 1.342453679581834924, -7.902645620902536194, 12.51077660954462978 ) ) ;
#11791 =( BOUNDED_SURFACE ( )  B_SPLINE_SURFACE ( 3, 1, ( 
 ( #9173, #4779 ),
 ( #17879, #16451 ),
 ( #16901, #8303 ),
 ( #5056, #3807 ) ),
 .UNSPECIFIED., .F., .F., .T. ) 
 B_SPLINE_SURFACE_WITH_KNOTS ( ( 4, 4 ),
 ( 2, 2 ),
 ( 0.000000000000000000, 1.000000000000000000 ),
 ( 0.000000000000000000, 1.000000000000000000 ),
 .UNSPECIFIED. ) 
 GEOMETRIC_REPRESENTATION_ITEM ( )  RATIONAL_B_SPLINE_SURFACE ( (
 ( 1.000000000000000000, 1.000000000000000000),
 ( 0.7792777138730158093, 0.9689936506012928330),
 ( 0.7792777138730158093, 0.9689936506012928330),
 ( 1.000000000000000000, 1.000000000000000000) ) ) 
 REPRESENTATION_ITEM ( '' )  SURFACE ( )  );
#11792 = CARTESIAN_POINT ( 'NONE',  ( 0.4862570985993235340, 5.003653737315670647, -12.97920246947874112 ) ) ;
#11793 = EDGE_LOOP ( 'NONE', ( #7795, #13409, #8754, #13611 ) ) ;
#11794 = ORIENTED_EDGE ( 'NONE', *, *, #8814, .F. ) ;
#11795 = CARTESIAN_POINT ( 'NONE',  ( 16.56872352241294521, 0.01027347319884366721, 0.001821578298043820656 ) ) ;
#11796 = EDGE_LOOP ( 'NONE', ( #12654, #9641, #5895, #16437 ) ) ;
#11797 = CARTESIAN_POINT ( 'NONE',  ( 16.56822296793089322, 0.003834730849371879857, 0.009385634690642069913 ) ) ;
#11798 = EDGE_LOOP ( 'NONE', ( #7961, #12730, #18563, #15479 ) ) ;
#11799 = LINE ( 'NONE', #11895, #7014 ) ;
#11800 = CARTESIAN_POINT ( 'NONE',  ( 0.3137051932979792457, -13.20008686438103140, -3.805684345189927154 ) ) ;
#11801 = CARTESIAN_POINT ( 'NONE',  ( 16.57778382496167424, -0.01354073047775762942, -0.006312874906843820091 ) ) ;
#11802 = FACE_OUTER_BOUND ( 'NONE', #14506, .T. ) ;
#11803 = CARTESIAN_POINT ( 'NONE',  ( 2.750000000000000000, 0.000000000000000000, 2.699999999999999734 ) ) ;
#11804 = CARTESIAN_POINT ( 'NONE',  ( 0.4754618798421162973, -7.564402563418551217, 11.68486377711963975 ) ) ;
#11805 = CARTESIAN_POINT ( 'NONE',  ( 1.342453679581834924, -9.456403821038877666, 11.38190519890850183 ) ) ;
#11806 = EDGE_CURVE ( 'NONE', #15560, #3963, #8697, .T. ) ;
#11807 = CARTESIAN_POINT ( 'NONE',  ( 1.918918678667047129, 4.466049546133911363, 11.69059232068580556 ) ) ;
#11808 = AXIS2_PLACEMENT_3D ( 'NONE', #12528, #18363, #11112 ) ;
#11809 = CARTESIAN_POINT ( 'NONE',  ( 6.000000000000000888, 17.00000000000000000, 3.000000000000000000 ) ) ;
#11810 = VECTOR ( 'NONE', #12283, 1000.000000000000000 ) ;
#11811 = CARTESIAN_POINT ( 'NONE',  ( 1.846138399168762101, 7.646096044340033870, -9.815003036200328879 ) ) ;
#11812 = CIRCLE ( 'NONE', #4486, 5.000000000000000000 ) ;
#11813 = LINE ( 'NONE', #10376, #6942 ) ;
#11814 = CARTESIAN_POINT ( 'NONE',  ( 2.636624412716062515, -6.973567714909003179, -14.46769361191335790 ) ) ;
#11815 = VERTEX_POINT ( 'NONE', #7182 ) ;
#11816 = B_SPLINE_CURVE_WITH_KNOTS ( 'NONE', 3,
 ( #13862, #11012, #18353, #780, #17024, #12609 ),
 .UNSPECIFIED., .F., .F.,
 ( 4, 2, 4 ),
 ( 4.240893905418535831E-17, 0.0002014099069817287303, 0.0004028198139634150141 ),
 .UNSPECIFIED. ) ;
#11817 = AXIS2_PLACEMENT_3D ( 'NONE', #8926, #13323, #13420 ) ;
#11818 = ORIENTED_EDGE ( 'NONE', *, *, #12847, .F. ) ;
#11819 = EDGE_LOOP ( 'NONE', ( #12077, #1030, #18782, #12062 ) ) ;
#11820 = ORIENTED_EDGE ( 'NONE', *, *, #1397, .F. ) ;
#11821 = CARTESIAN_POINT ( 'NONE',  ( 1.959212340397943120, -9.750290364083578964, -7.909199412631276793 ) ) ;
#11822 = CARTESIAN_POINT ( 'NONE',  ( 16.56679352167444819, -0.006618561353600137254, -0.006526964904752322223 ) ) ;
#11823 = CARTESIAN_POINT ( 'NONE',  ( 0.4754618798421162973, -12.98792082933640835, -5.007009103465388300 ) ) ;
#11824 = EDGE_LOOP ( 'NONE', ( #9043, #2952, #4427, #15986 ) ) ;
#11825 = CARTESIAN_POINT ( 'NONE',  ( 2.369999999999999662, 0.000000000000000000, 0.000000000000000000 ) ) ;
#11826 = VECTOR ( 'NONE', #1626, 1000.000000000000000 ) ;
#11827 = DIRECTION ( 'NONE',  ( 0.000000000000000000, 0.000000000000000000, 1.000000000000000000 ) ) ;
#11828 = PLANE ( 'NONE',  #3947 ) ;
#11829 = CARTESIAN_POINT ( 'NONE',  ( 0.3142011359265305392, 8.382042760265909109, 10.88514493056445076 ) ) ;
#11830 = EDGE_CURVE ( 'NONE', #18306, #18321, #18404, .T. ) ;
#11831 = EDGE_CURVE ( 'NONE', #16063, #15590, #4697, .T. ) ;
#11832 = CARTESIAN_POINT ( 'NONE',  ( 1.847412631396504690, 0.04315047898452520347, -12.44294644888238643 ) ) ;
#11833 = CARTESIAN_POINT ( 'NONE',  ( 0.3058872367615230181, -11.46514199369352482, -7.578326039752732335 ) ) ;
#11834 = EDGE_CURVE ( 'NONE', #15279, #1391, #4306, .T. ) ;
#11835 = CARTESIAN_POINT ( 'NONE',  ( 0.3150692679895942816, -11.02465386701222805, -8.199139630396127032 ) ) ;
#11836 = CARTESIAN_POINT ( 'NONE',  ( 0.3150692679895937820, -7.951395415075003470, -11.20465057551034604 ) ) ;
#11837 = CIRCLE ( 'NONE', #3597, 5.000000000000000000 ) ;
#11838 = VERTEX_POINT ( 'NONE', #14524 ) ;
#11839 = ORIENTED_EDGE ( 'NONE', *, *, #2636, .F. ) ;
#11840 = EDGE_LOOP ( 'NONE', ( #7894, #9274, #7374, #10705 ) ) ;
#11841 = ORIENTED_EDGE ( 'NONE', *, *, #5321, .T. ) ;
#11842 = CARTESIAN_POINT ( 'NONE',  ( 1.845755665168035575, 9.776700214454821847, 7.694641135843453661 ) ) ;
#11843 = ORIENTED_EDGE ( 'NONE', *, *, #3294, .F. ) ;
#11844 = CARTESIAN_POINT ( 'NONE',  ( 0.3058872367615226295, -11.46514199369363318, 7.578326039752564469 ) ) ;
#11845 = CARTESIAN_POINT ( 'NONE',  ( 0.3170788640506440603, -13.02120094575825249, -4.392045232375947350 ) ) ;
#11846 = CARTESIAN_POINT ( 'NONE',  ( 1.474209205587600649E-14, -8.013167318348349610, 12.51316734529529562 ) ) ;
#11847 = CARTESIAN_POINT ( 'NONE',  ( 1.846138399168762101, -0.4167076046094680408, -12.43476674860266940 ) ) ;
#11848 = VERTEX_POINT ( 'NONE', #14339 ) ;
#11849 = CARTESIAN_POINT ( 'NONE',  ( -1.391363329066502619, 7.500000000000000000, -14.80343650618309326 ) ) ;
#11850 = CIRCLE ( 'NONE', #16447, 7.000000000000000000 ) ;
#11851 = SPHERICAL_SURFACE ( 'NONE', #8968, 5.000000000000000000 ) ;
#11852 = DIRECTION ( 'NONE',  ( 0.000000000000000000, 1.000000000000000000, 0.000000000000000000 ) ) ;
#11853 = CARTESIAN_POINT ( 'NONE',  ( 0.4754618798421171855, 7.564402563418640035, -11.68486377711958291 ) ) ;
#11854 = DIRECTION ( 'NONE',  ( -0.9034263296138842492, 0.000000000000000000, -0.4287433579198461908 ) ) ;
#11855 = AXIS2_PLACEMENT_3D ( 'NONE', #18370, #5458, #17120 ) ;
#11856 = CARTESIAN_POINT ( 'NONE',  ( 1.136782529653004747, -40.00000000000000000, 6.000000000000000000 ) ) ;
#11857 = ORIENTED_EDGE ( 'NONE', *, *, #8921, .T. ) ;
#11858 = ADVANCED_FACE ( 'NONE', ( #1441 ), #13092, .F. ) ;
#11859 = CARTESIAN_POINT ( 'NONE',  ( 1.846138399168762101, -10.30487220521574976, 6.971848976710974810 ) ) ;
#11861 = ORIENTED_EDGE ( 'NONE', *, *, #10072, .T. ) ;
#11860 = CARTESIAN_POINT ( 'NONE',  ( 1.847034903785825799, 0.2299360331935915713, -12.44051878787772480 ) ) ;
#11862 = CARTESIAN_POINT ( 'NONE',  ( -108.4421517486958351, -82.42962774651277869, -83.76786890419475640 ) ) ;
#11863 = CARTESIAN_POINT ( 'NONE',  ( 16.56782317627811096, -0.003357783021327304974, 0.009228812961909584403 ) ) ;
#11864 = B_SPLINE_CURVE_WITH_KNOTS ( 'NONE', 3,
 ( #5645, #15886, #13115, #219 ),
 .UNSPECIFIED., .F., .F.,
 ( 4, 4 ),
 ( 9.796581096179191873E-17, 0.002004993803842611885 ),
 .UNSPECIFIED. ) ;
#11865 = ORIENTED_EDGE ( 'NONE', *, *, #6920, .F. ) ;
#11866 = CARTESIAN_POINT ( 'NONE',  ( 2.705023505549862595, -7.115606223895247773, 11.23800170568054568 ) ) ;
#11867 = UNCERTAINTY_MEASURE_WITH_UNIT (LENGTH_MEASURE( 1.000000000000000082E-05 ), #18471, 'distance_accuracy_value', 'NONE');
#11868 = CARTESIAN_POINT ( 'NONE',  ( 3.648056509801858027, -7.500000000000000888, -16.29094785500087994 ) ) ;
#11869 =( BOUNDED_SURFACE ( )  B_SPLINE_SURFACE ( 3, 1, ( 
 ( #16580, #2470 ),
 ( #14238, #14135 ),
 ( #15041, #9408 ),
 ( #2055, #18536 ) ),
 .UNSPECIFIED., .F., .F., .T. ) 
 B_SPLINE_SURFACE_WITH_KNOTS ( ( 4, 4 ),
 ( 2, 2 ),
 ( 0.000000000000000000, 1.000000000000000000 ),
 ( 0.000000000000000000, 1.000000000000000000 ),
 .UNSPECIFIED. ) 
 GEOMETRIC_REPRESENTATION_ITEM ( )  RATIONAL_B_SPLINE_SURFACE ( (
 ( 1.000000000000000000, 1.000000000000000000),
 ( 0.9933953342250438912, 0.8357391271907739227),
 ( 0.9933953342250438912, 0.8357391271907739227),
 ( 1.000000000000000000, 1.000000000000000000) ) ) 
 REPRESENTATION_ITEM ( '' )  SURFACE ( )  );
#11870 = VERTEX_POINT ( 'NONE', #1242 ) ;
#11871 = FACE_OUTER_BOUND ( 'NONE', #2878, .T. ) ;
#11872 = DIRECTION ( 'NONE',  ( 0.000000000000000000, 0.000000000000000000, -1.000000000000000000 ) ) ;
#11873 = CARTESIAN_POINT ( 'NONE',  ( 3.074695600507272086, -2.093687500612061658, 15.41438262616222765 ) ) ;
#11874 = CARTESIAN_POINT ( 'NONE',  ( 0.4862570985993235340, -10.79774104611366781, -8.769551628660854803 ) ) ;
#11875 = ADVANCED_FACE ( 'NONE', ( #16054 ), #2948, .T. ) ;
#11876 = EDGE_CURVE ( 'NONE', #17620, #2287, #12900, .T. ) ;
#11877 = CARTESIAN_POINT ( 'NONE',  ( -27.50000000000000711, -12.50000000000000178, 0.000000000000000000 ) ) ;
#11878 = DIRECTION ( 'NONE',  ( 1.000000000000000000, 0.000000000000000000, 0.000000000000000000 ) ) ;
#11879 = ADVANCED_FACE ( 'NONE', ( #17589 ), #7441, .T. ) ;
#11880 = FACE_OUTER_BOUND ( 'NONE', #14984, .T. ) ;
#11881 = CARTESIAN_POINT ( 'NONE',  ( 16.57210152137263393, 0.01402404281922921964, -0.003862718596009325888 ) ) ;
#11882 = FACE_OUTER_BOUND ( 'NONE', #18623, .T. ) ;
#11883 = VERTEX_POINT ( 'NONE', #4502 ) ;
#11884 = CARTESIAN_POINT ( 'NONE',  ( 0.3148213771069381384, -4.463459503829087183, 12.99360322443201277 ) ) ;
#11885 = CARTESIAN_POINT ( 'NONE',  ( 0.3170788640506440603, -11.20690911610909168, 7.952793437297537515 ) ) ;
#11886 = VERTEX_POINT ( 'NONE', #3036 ) ;
#11887 = ORIENTED_EDGE ( 'NONE', *, *, #15789, .F. ) ;
#11888 = CARTESIAN_POINT ( 'NONE',  ( 15.00000000000000711, -14.99999999999999645, 7.000000000000000000 ) ) ;
#11889 = ORIENTED_EDGE ( 'NONE', *, *, #6422, .F. ) ;
#11890 = CARTESIAN_POINT ( 'NONE',  ( 2.002547531651519996, -3.242439124566736997, 12.17374746633577232 ) ) ;
#11891 = VECTOR ( 'NONE', #9243, 1000.000000000000000 ) ;
#11892 = AXIS2_PLACEMENT_3D ( 'NONE', #9582, #8898, #4322 ) ;
#11893 = ORIENTED_EDGE ( 'NONE', *, *, #10701, .F. ) ;
#11894 = ADVANCED_FACE ( 'NONE', ( #15443 ), #9568, .F. ) ;
#11895 = CARTESIAN_POINT ( 'NONE',  ( 1.560000000000000053, 0.8660254037844389297, 1.500000000000000000 ) ) ;
#11896 = FACE_OUTER_BOUND ( 'NONE', #16212, .T. ) ;
#11897 = DIRECTION ( 'NONE',  ( -1.000000000000000000, -0.000000000000000000, -0.000000000000000000 ) ) ;
#11898 = CARTESIAN_POINT ( 'NONE',  ( 0.4385251269669960816, -8.732456510146150208, 10.76637725024249193 ) ) ;
#11899 = EDGE_CURVE ( 'NONE', #15560, #348, #8070, .T. ) ;
#11900 = FACE_OUTER_BOUND ( 'NONE', #4820, .T. ) ;
#11901 = CARTESIAN_POINT ( 'NONE',  ( 0.4862570985993235340, 10.79774104611385965, -8.769551628660616771 ) ) ;
#11902 = B_SPLINE_CURVE_WITH_KNOTS ( 'NONE', 3,
 ( #2543, #12965, #8667, #18796, #941, #3908, #17367, #4283, #2454, #10106, #15933, #8306, #16131 ),
 .UNSPECIFIED., .F., .F.,
 ( 4, 3, 3, 3, 4 ),
 ( 1.734723475976807094E-18, 0.0002299804304191470643, 0.0004599608082120238165, 0.0006467586077648016917, 0.0008336169836825990491 ),
 .UNSPECIFIED. ) ;
#11903 = CARTESIAN_POINT ( 'NONE',  ( 0.3939822652208134768, -3.598529276937167953, -13.34132036472940896 ) ) ;
#11904 = DIRECTION ( 'NONE',  ( 0.000000000000000000, 0.000000000000000000, -1.000000000000000000 ) ) ;
#11905 = CARTESIAN_POINT ( 'NONE',  ( 2.747332970342022840, 7.289199830147106596, 14.63517873738950037 ) ) ;
#11906 = CARTESIAN_POINT ( 'NONE',  ( 0.4385251269669945273, -7.540955776459655091, -11.63205320541531052 ) ) ;
#11907 = DIRECTION ( 'NONE',  ( -0.000000000000000000, -0.000000000000000000, 1.000000000000000000 ) ) ;
#11908 = CARTESIAN_POINT ( 'NONE',  ( 16.56822296793089322, -0.006547366384936689071, -0.007741272030791150442 ) ) ;
#11909 = ORIENTED_EDGE ( 'NONE', *, *, #14876, .F. ) ;
#11910 = ORIENTED_EDGE ( 'NONE', *, *, #6516, .F. ) ;
#11911 = ORIENTED_EDGE ( 'NONE', *, *, #9268, .F. ) ;
#11912 = ORIENTED_EDGE ( 'NONE', *, *, #8274, .T. ) ;
#11913 = B_SPLINE_CURVE_WITH_KNOTS ( 'NONE', 3,
 ( #13487, #6233, #10637, #4900, #13299, #6045 ),
 .UNSPECIFIED., .F., .F.,
 ( 4, 2, 4 ),
 ( 4.256846838097967453E-17, 0.0002014099069817298958, 0.0004028198139634172367 ),
 .UNSPECIFIED. ) ;
#11914 = EDGE_CURVE ( 'NONE', #18549, #1302, #1453, .T. ) ;
#11915 = CARTESIAN_POINT ( 'NONE',  ( 16.57605080000000086, 0.000000000000000000, 0.000000000000000000 ) ) ;
#11916 = CARTESIAN_POINT ( 'NONE',  ( 16.56782317627811096, -0.009814734722106369796, 0.0003415813796014346851 ) ) ;
#11917 = CARTESIAN_POINT ( 'NONE',  ( 1.845755665166725290, 0.4784952423730285953, -12.43231320373360660 ) ) ;
#11918 = ORIENTED_EDGE ( 'NONE', *, *, #14975, .F. ) ;
#11919 = DIRECTION ( 'NONE',  ( 0.000000000000000000, 0.000000000000000000, 1.000000000000000000 ) ) ;
#11920 = DIRECTION ( 'NONE',  ( 0.000000000000000000, 0.000000000000000000, 1.000000000000000000 ) ) ;
#11921 = CARTESIAN_POINT ( 'NONE',  ( 16.56872352241294521, -0.004564908236400030961, 0.009382111268607351909 ) ) ;
#11922 = CARTESIAN_POINT ( 'NONE',  ( 2.636624412716062960, -2.161493821598612808, -15.91454522070331912 ) ) ;
#11923 = CARTESIAN_POINT ( 'NONE',  ( 2.002547531651519996, -4.532360870844247991, -11.75462648437106417 ) ) ;
#11924 = CARTESIAN_POINT ( 'NONE',  ( 0.4862570985993252548, -5.003653737315580052, 12.97920246947877665 ) ) ;
#11925 = CARTESIAN_POINT ( 'NONE',  ( 0.3145734862173208413, -10.93207848441427643, -8.321353293018953323 ) ) ;
#11926 = DIRECTION ( 'NONE',  ( 1.000000000000000000, 0.000000000000000000, 0.000000000000000000 ) ) ;
#11927 = CARTESIAN_POINT ( 'NONE',  ( 0.3145734862173253377, 4.535879238195112073, -12.96846406299301258 ) ) ;
#11928 = VERTEX_POINT ( 'NONE', #16796 ) ;
#11929 = B_SPLINE_CURVE_WITH_KNOTS ( 'NONE', 3,
 ( #330, #9022, #4824, #11987 ),
 .UNSPECIFIED., .F., .F.,
 ( 4, 4 ),
 ( 0.000000000000000000, 0.002004993803840905784 ),
 .UNSPECIFIED. ) ;
#11930 = VERTEX_POINT ( 'NONE', #7665 ) ;
#11931 = EDGE_LOOP ( 'NONE', ( #7861, #13622, #13977, #5773 ) ) ;
#11932 = APPLICATION_CONTEXT ( 'automotive_design' ) ;
#11933 = ORIENTED_EDGE ( 'NONE', *, *, #5439, .F. ) ;
#11934 = FACE_OUTER_BOUND ( 'NONE', #4429, .T. ) ;
#11935 = EDGE_CURVE ( 'NONE', #6348, #6138, #4886, .T. ) ;
#11936 = VERTEX_POINT ( 'NONE', #17786 ) ;
#11937 = EDGE_CURVE ( 'NONE', #2927, #14774, #15818, .T. ) ;
#11938 = EDGE_CURVE ( 'NONE', #8583, #14839, #921, .T. ) ;
#11939 = DIRECTION ( 'NONE',  ( -1.000000000000000000, -0.000000000000000000, -0.000000000000000000 ) ) ;
#11940 = AXIS2_PLACEMENT_3D ( 'NONE', #17790, #4693, #6320 ) ;
#11941 = CARTESIAN_POINT ( 'NONE',  ( 1.846138399168762101, 10.30487220521580305, -6.971848976710897539 ) ) ;
#11942 = CARTESIAN_POINT ( 'NONE',  ( 0.4862570985993235340, -8.769551628660655851, -10.79774104611382946 ) ) ;
#11943 = FACE_OUTER_BOUND ( 'NONE', #1605, .T. ) ;
#11944 = VERTEX_POINT ( 'NONE', #5224 ) ;
#11945 = CARTESIAN_POINT ( 'NONE',  ( 2.705023505549867036, 12.88681800078732387, 3.294610156755938934 ) ) ;
#11946 = CARTESIAN_POINT ( 'NONE',  ( -6.538348415311010520, -2.500000000000000444, -12.00000000000000000 ) ) ;
#11947 = DIRECTION ( 'NONE',  ( 0.000000000000000000, 0.000000000000000000, -1.000000000000000000 ) ) ;
#11948 = CARTESIAN_POINT ( 'NONE',  ( 1.847380140988738262, -10.00162556679656234, 7.402792205949069171 ) ) ;
#11949 = CARTESIAN_POINT ( 'NONE',  ( 2.636624412714134280, 2.862162146984768896, 15.80357026013147426 ) ) ;
#11950 = CARTESIAN_POINT ( 'NONE',  ( 3.377929128793398572, 3.070552481925057364, -13.64476897106781017 ) ) ;
#11951 = B_SPLINE_CURVE_WITH_KNOTS ( 'NONE', 3,
 ( #9522, #2350, #16608, #15347, #3409, #9439 ),
 .UNSPECIFIED., .F., .F.,
 ( 4, 2, 4 ),
 ( 0.000000000000000000, 0.001656992708822828484, 0.003313985417645657836 ),
 .UNSPECIFIED. ) ;
#11952 = CARTESIAN_POINT ( 'NONE',  ( 2.002547531651519996, 7.942910686618173344, 9.778737580845726640 ) ) ;
#11953 = ORIENTED_EDGE ( 'NONE', *, *, #8274, .F. ) ;
#11954 = CIRCLE ( 'NONE', #14380, 14.54644660717763927 ) ;
#11955 = DIRECTION ( 'NONE',  ( 0.000000000000000000, 0.000000000000000000, -1.000000000000000000 ) ) ;
#11957 = ORIENTED_EDGE ( 'NONE', *, *, #2325, .T. ) ;
#11956 = CARTESIAN_POINT ( 'NONE',  ( -61.35602477868047799, -15.00000000000000711, 3.000000000000000000 ) ) ;
#11958 = CARTESIAN_POINT ( 'NONE',  ( 2.002547531651519996, 12.57989064830759496, 0.6781519942172178350 ) ) ;
#11959 = DIRECTION ( 'NONE',  ( 0.000000000000000000, 0.000000000000000000, 1.000000000000000000 ) ) ;
#11960 = ORIENTED_EDGE ( 'NONE', *, *, #17496, .F. ) ;
#11961 = DIRECTION ( 'NONE',  ( -1.000000000000000000, -0.000000000000000000, -0.000000000000000000 ) ) ;
#11962 = PRODUCT ( 'spacer', 'spacer', '', ( #10855 ) ) ;
#11963 = CARTESIAN_POINT ( 'NONE',  ( 2.953963787679646735, -6.378445150919258566, -12.00000001548996487 ) ) ;
#11964 = ORIENTED_EDGE ( 'NONE', *, *, #7829, .T. ) ;
#11965 = CARTESIAN_POINT ( 'NONE',  ( 1.846138399168762101, 4.238866729160568170, -11.69739621335917690 ) ) ;
#11966 = FACE_OUTER_BOUND ( 'NONE', #8003, .T. ) ;
#11967 = EDGE_CURVE ( 'NONE', #10086, #2296, #741, .T. ) ;
#11968 = EDGE_CURVE ( 'NONE', #14367, #400, #18707, .T. ) ;
#11969 = CARTESIAN_POINT ( 'NONE',  ( 8.522092701127531811, -6.722964936702084948, -1.786985377232103600 ) ) ;
#11970 = CARTESIAN_POINT ( 'NONE',  ( 11.50000000000000178, 0.000000000000000000, 10.49999999999999822 ) ) ;
#11971 = ORIENTED_EDGE ( 'NONE', *, *, #7475, .T. ) ;
#11972 = CONICAL_SURFACE ( 'NONE', #14701, 14.54644660717763927, 0.8559913436420816257 ) ;
#11973 = ADVANCED_FACE ( 'NONE', ( #8197 ), #655, .F. ) ;
#11974 = CARTESIAN_POINT ( 'NONE',  ( 0.000000000000000000, 4.769696007084728073, -1.500000000000000000 ) ) ;
#11975 = B_SPLINE_CURVE_WITH_KNOTS ( 'NONE', 3,
 ( #16948, #3850, #9681, #15506, #11034, #9765 ),
 .UNSPECIFIED., .F., .F.,
 ( 4, 2, 4 ),
 ( 3.527508043940425264E-17, 0.0001825746017570591031, 0.0003651492035140829697 ),
 .UNSPECIFIED. ) ;
#11976 = CARTESIAN_POINT ( 'NONE',  ( 16.56782317627811096, -0.005492611183757366636, 0.008141063682853383679 ) ) ;
#11977 = DIRECTION ( 'NONE',  ( -1.000000000000000000, 0.000000000000000000, -0.000000000000000000 ) ) ;
#11978 = DIRECTION ( 'NONE',  ( 1.000000000000000000, 0.000000000000000000, 0.000000000000000000 ) ) ;
#11979 = ORIENTED_EDGE ( 'NONE', *, *, #6371, .T. ) ;
#11980 = CARTESIAN_POINT ( 'NONE',  ( 0.3142011359265320380, -3.879426116491784260, 13.17934269988456819 ) ) ;
#11981 = CARTESIAN_POINT ( 'NONE',  ( 0.4384471787762824757, -13.84291427302852107, 0.7363690479465839767 ) ) ;
#11982 =( BOUNDED_SURFACE ( )  B_SPLINE_SURFACE ( 3, 1, ( 
 ( #4742, #1780 ),
 ( #1877, #6374 ),
 ( #10670, #13237 ),
 ( #16504, #18026 ) ),
 .UNSPECIFIED., .F., .F., .T. ) 
 B_SPLINE_SURFACE_WITH_KNOTS ( ( 4, 4 ),
 ( 2, 2 ),
 ( 0.000000000000000000, 1.000000000000000000 ),
 ( 0.000000000000000000, 1.000000000000000000 ),
 .UNSPECIFIED. ) 
 GEOMETRIC_REPRESENTATION_ITEM ( )  RATIONAL_B_SPLINE_SURFACE ( (
 ( 1.000000000000000000, 1.000000000000000000),
 ( 0.9593108457356467333, 0.9995965569486454649),
 ( 0.9593108457356467333, 0.9995965569486454649),
 ( 1.000000000000000000, 1.000000000000000000) ) ) 
 REPRESENTATION_ITEM ( '' )  SURFACE ( )  );
#11983 = EDGE_LOOP ( 'NONE', ( #17492, #1011, #16615, #423, #15354, #6442 ) ) ;
#11984 = ORIENTED_EDGE ( 'NONE', *, *, #7806, .T. ) ;
#11985 = CARTESIAN_POINT ( 'NONE',  ( 1.846138399168762101, -0.4167076046096411246, 12.43476674860266407 ) ) ;
#11986 = ORIENTED_EDGE ( 'NONE', *, *, #16857, .T. ) ;
#11987 = CARTESIAN_POINT ( 'NONE',  ( 2.636624412717140764, -2.862162146982851763, -15.80357026013259514 ) ) ;
#11988 = CIRCLE ( 'NONE', #7408, 16.06066017081991149 ) ;
#11989 = EDGE_CURVE ( 'NONE', #15782, #1651, #3696, .T. ) ;
#11990 = ORIENTED_EDGE ( 'NONE', *, *, #10895, .T. ) ;
#11991 = ADVANCED_FACE ( 'NONE', ( #11067 ), #2615, .F. ) ;
#11992 = EDGE_CURVE ( 'NONE', #11620, #10419, #17156, .T. ) ;
#11993 = DIRECTION ( 'NONE',  ( -1.913297951445007868E-16, 1.000000000000000000, 0.000000000000000000 ) ) ;
#11994 = CARTESIAN_POINT ( 'NONE',  ( 2.002547531651519996, -12.57989064830760206, 0.6781519942171299054 ) ) ;
#11995 = CIRCLE ( 'NONE', #5270, 4.750000000000000000 ) ;
#11996 = CARTESIAN_POINT ( 'NONE',  ( 0.3137051932979792457, -0.4596302728640728752, 13.73004976592201842 ) ) ;
#11997 = DIRECTION ( 'NONE',  ( 1.000000000000000000, 0.000000000000000000, 0.000000000000000000 ) ) ;
#11998 = ADVANCED_FACE ( 'NONE', ( #6847 ), #16784, .F. ) ;
#11999 =( NAMED_UNIT ( * ) SI_UNIT ( $, .STERADIAN. ) SOLID_ANGLE_UNIT ( ) );
#12000 = FACE_OUTER_BOUND ( 'NONE', #18368, .T. ) ;
#12001 = CARTESIAN_POINT ( 'NONE',  ( 1.977436885026784941, 6.153171729169462090, -14.12046670317587704 ) ) ;
#12002 = CARTESIAN_POINT ( 'NONE',  ( 6.538348415311010520, 7.499999999999999112, -16.99999999999999645 ) ) ;
#12003 = CARTESIAN_POINT ( 'NONE',  ( 0.3145734862173251711, 13.73540602248380971, 0.3064017202075832724 ) ) ;
#12004 = EDGE_CURVE ( 'NONE', #14287, #4150, #17640, .T. ) ;
#12005 = CARTESIAN_POINT ( 'NONE',  ( -25.00000000000000000, 2.499999999999998668, -17.00000000000000000 ) ) ;
#12006 = CARTESIAN_POINT ( 'NONE',  ( 2.636624412714236865, 0.000000000000000000, 0.000000000000000000 ) ) ;
#12007 = ORIENTED_EDGE ( 'NONE', *, *, #9429, .T. ) ;
#12008 = VECTOR ( 'NONE', #15348, 1000.000000000000000 ) ;
#12009 = ORIENTED_EDGE ( 'NONE', *, *, #13925, .T. ) ;
#12010 = VERTEX_POINT ( 'NONE', #17070 ) ;
#12011 = EDGE_LOOP ( 'NONE', ( #4453, #18528, #255, #15888 ) ) ;
#12012 = CARTESIAN_POINT ( 'NONE',  ( 20.00000000000000711, -24.99999999999999645, 3.000000000000000000 ) ) ;
#12013 = CARTESIAN_POINT ( 'NONE',  ( 16.56872352241294521, -0.01027347319884365333, -0.001821578298043897851 ) ) ;
#12014 = CARTESIAN_POINT ( 'NONE',  ( 16.56782317627811096, 0.009439921864426886397, -0.002708056627498675335 ) ) ;
#12015 = CARTESIAN_POINT ( 'NONE',  ( 0.3308579732646998450, 13.74211098745269766, 0.5950689966504839612 ) ) ;
#12016 = CARTESIAN_POINT ( 'NONE',  ( 1.918918678667072442, -12.49849921341423276, 0.6348738215464800883 ) ) ;
#12017 = DIRECTION ( 'NONE',  ( 0.000000000000000000, 0.000000000000000000, 1.000000000000000000 ) ) ;
#12018 = CARTESIAN_POINT ( 'NONE',  ( 1.254009781011619307, -7.789615163754444183, 12.44229282923071445 ) ) ;
#12019 = CARTESIAN_POINT ( 'NONE',  ( 16.56782317627811096, 0.0003415813796006246777, -0.009814734722107084502 ) ) ;
#12020 = AXIS2_PLACEMENT_3D ( 'NONE', #4219, #7278, #2843 ) ;
#12021 = ADVANCED_FACE ( 'NONE', ( #5312 ), #5763, .F. ) ;
#12022 = AXIS2_PLACEMENT_3D ( 'NONE', #5414, #17079, #2531 ) ;
#12023 = CARTESIAN_POINT ( 'NONE',  ( 1.846524061778019199, 0.3544704288994222074, -12.43723828841088164 ) ) ;
#12024 = CARTESIAN_POINT ( 'NONE',  ( 1.846138399168762101, -9.815003036200353748, -7.646096044340000120 ) ) ;
#12025 = CARTESIAN_POINT ( 'NONE',  ( 0.3137051932979792457, -12.91601973349266963, -4.679953077377624560 ) ) ;
#12026 = DIRECTION ( 'NONE',  ( 1.000000000000000000, 0.000000000000000000, 0.000000000000000000 ) ) ;
#12027 = CARTESIAN_POINT ( 'NONE',  ( 0.3137051932979775248, 3.805684345189972895, -13.20008686438101719 ) ) ;
#12028 = ADVANCED_FACE ( 'NONE', ( #18402 ), #2577, .F. ) ;
#12029 = ORIENTED_EDGE ( 'NONE', *, *, #18640, .F. ) ;
#12030 = ORIENTED_EDGE ( 'NONE', *, *, #17968, .T. ) ;
#12031 = ORIENTED_EDGE ( 'NONE', *, *, #11160, .T. ) ;
#12032 = VERTEX_POINT ( 'NONE', #18678 ) ;
#12033 = DIRECTION ( 'NONE',  ( 1.000000000000000000, 0.000000000000000000, 0.000000000000000000 ) ) ;
#12034 = CARTESIAN_POINT ( 'NONE',  ( 0.4862570985993235340, -0.7479633556563419772, 13.89016912371017121 ) ) ;
#12035 = VECTOR ( 'NONE', #12321, 1000.000000000000000 ) ;
#12036 = PRESENTATION_LAYER_ASSIGNMENT (  '', '', ( #14763 ) ) ;
#12037 = DIRECTION ( 'NONE',  ( -1.000000000000000000, -0.000000000000000000, -0.000000000000000000 ) ) ;
#12038 = CARTESIAN_POINT ( 'NONE',  ( 0.4754618798421162973, 5.007009103465249744, 12.98792082933646341 ) ) ;
#12039 = PRODUCT_DEFINITION_FORMATION_WITH_SPECIFIED_SOURCE ( 'ANY', '', #10755, .NOT_KNOWN. ) ;
#12040 = LINE ( 'NONE', #17778, #11154 ) ;
#12041 = VERTEX_POINT ( 'NONE', #8286 ) ;
#12042 = CARTESIAN_POINT ( 'NONE',  ( -4.478293880065214339, 7.500000000000000888, -16.64373187125687181 ) ) ;
#12043 = CARTESIAN_POINT ( 'NONE',  ( 0.3151926232592501265, 13.09050869763092884, 4.172630140040843649 ) ) ;
#12044 = CARTESIAN_POINT ( 'NONE',  ( 16.58200780006414732, 0.009393638146078525306, 0.006043560077721743008 ) ) ;
#12045 = CARTESIAN_POINT ( 'NONE',  ( 16.56872352241294521, -0.007240717549633937135, 0.007512283835805527027 ) ) ;
#12046 = CARTESIAN_POINT ( 'NONE',  ( 3.950837973638676281, -12.81214529934970336, -6.888253895133431115 ) ) ;
#12047 = ADVANCED_FACE ( 'NONE', ( #5578 ), #5165, .F. ) ;
#12048 = CARTESIAN_POINT ( 'NONE',  ( 2.636624412714994037, -14.46769361191274328, -6.973567714907344950 ) ) ;
#12049 = EDGE_CURVE ( 'NONE', #2427, #15029, #8372, .T. ) ;
#12050 = EDGE_CURVE ( 'NONE', #2337, #7261, #4069, .T. ) ;
#12051 = ORIENTED_EDGE ( 'NONE', *, *, #6850, .T. ) ;
#12052 = CARTESIAN_POINT ( 'NONE',  ( 0.3137051932979775248, 0.4596302728639756197, 13.73004976592202198 ) ) ;
#12054 = ORIENTED_EDGE ( 'NONE', *, *, #16782, .F. ) ;
#12053 = DIRECTION ( 'NONE',  ( -1.000000000000000000, 3.469446951953611033E-15, 0.000000000000000000 ) ) ;
#12055 = CARTESIAN_POINT ( 'NONE',  ( -2.179449471770337432, -4.500000000000000000, -6.000000000000000000 ) ) ;
#12056 = CONICAL_SURFACE ( 'NONE', #3802, 14.54644660717763927, 0.8559913436420816257 ) ;
#12057 = VECTOR ( 'NONE', #14025, 1000.000000000000114 ) ;
#12058 = CARTESIAN_POINT ( 'NONE',  ( 0.3058872367615230181, 13.72992299905060065, -0.6080468242581438254 ) ) ;
#12059 = ORIENTED_EDGE ( 'NONE', *, *, #16689, .T. ) ;
#12060 = CARTESIAN_POINT ( 'NONE',  ( 8.438534575730034959, -4.221456476902624821, -5.415535776177568650 ) ) ;
#12061 = CARTESIAN_POINT ( 'NONE',  ( -1.454043889487635077, -7.499999999999869438, -13.09460583645939558 ) ) ;
#12062 = ORIENTED_EDGE ( 'NONE', *, *, #1729, .F. ) ;
#12063 = CARTESIAN_POINT ( 'NONE',  ( 3.950837973638676281, 10.05648675950141602, -10.51028938476206953 ) ) ;
#12064 = DIRECTION ( 'NONE',  ( -0.7635533937278216055, -0.6453904417649388714, 0.02138673900301666167 ) ) ;
#12065 = AXIS2_PLACEMENT_3D ( 'NONE', #17200, #4111, #12611 ) ;
#12066 = CARTESIAN_POINT ( 'NONE',  ( 1.861628059977342486, 4.358833901513207820, -11.66985327793194216 ) ) ;
#12067 = AXIS2_PLACEMENT_3D ( 'NONE', #11202, #3926, #13617 ) ;
#12068 = CARTESIAN_POINT ( 'NONE',  ( 0.4862570985993252548, 3.580942890621670482, 13.44146924561382583 ) ) ;
#12069 = AXIS2_PLACEMENT_3D ( 'NONE', #10408, #18059, #16539 ) ;
#12070 = ADVANCED_FACE ( 'NONE', ( #17539 ), #17616, .F. ) ;
#12071 = CARTESIAN_POINT ( 'NONE',  ( 1.959283090834840646, -6.829027319138321062, 10.53516775895158020 ) ) ;
#12072 = EDGE_CURVE ( 'NONE', #6854, #5564, #5868, .T. ) ;
#12073 = CARTESIAN_POINT ( 'NONE',  ( 0.4862570985993235340, -3.580942890621579444, -13.44146924561384537 ) ) ;
#12074 = EDGE_CURVE ( 'NONE', #14367, #10086, #11403, .T. ) ;
#12075 = LINE ( 'NONE', #13781, #5232 ) ;
#12077 = ORIENTED_EDGE ( 'NONE', *, *, #4987, .F. ) ;
#12076 = DIRECTION ( 'NONE',  ( -0.000000000000000000, -0.000000000000000000, 1.000000000000000000 ) ) ;
#12078 = CARTESIAN_POINT ( 'NONE',  ( -5.000000000000000000, 0.000000000000000000, 3.000000000000000000 ) ) ;
#12079 = STYLED_ITEM ( 'NONE', ( #18622 ), #9885 ) ;
#12080 = ORIENTED_EDGE ( 'NONE', *, *, #14495, .F. ) ;
#12081 = CARTESIAN_POINT ( 'NONE',  ( 0.3151930723728413875, -8.137566970826446422, 11.07033375389128871 ) ) ;
#12082 = CARTESIAN_POINT ( 'NONE',  ( 3.950837973638676281, -14.41405733518059229, -1.958075594453940971 ) ) ;
#12083 = AXIS2_PLACEMENT_3D ( 'NONE', #18795, #8576, #13063 ) ;
#12084 = EDGE_LOOP ( 'NONE', ( #16869, #393, #6606 ) ) ;
#12085 = EDGE_LOOP ( 'NONE', ( #16789, #837, #10614 ) ) ;
#12086 = CARTESIAN_POINT ( 'NONE',  ( 1.846138399168762101, -0.4167076046096411246, 12.43476674860266407 ) ) ;
#12087 = VERTEX_POINT ( 'NONE', #3287 ) ;
#12088 = CARTESIAN_POINT ( 'NONE',  ( 1.918921323896325193, 3.258415356426521026, 12.08297777410666285 ) ) ;
#12089 = ORIENTED_EDGE ( 'NONE', *, *, #6909, .F. ) ;
#12090 = CARTESIAN_POINT ( 'NONE',  ( 0.3142014840576499712, -13.73311050063163563, -0.3830336514510319090 ) ) ;
#12091 = CARTESIAN_POINT ( 'NONE',  ( 0.4862570985993235340, 13.89016912371017476, -0.7479633556562934604 ) ) ;
#12092 = DIRECTION ( 'NONE',  ( -0.000000000000000000, -0.000000000000000000, 1.000000000000000000 ) ) ;
#12093 = AXIS2_PLACEMENT_3D ( 'NONE', #7120, #12940, #5571 ) ;
#12094 = DIRECTION ( 'NONE',  ( 0.000000000000000000, 0.000000000000000000, 1.000000000000000000 ) ) ;
#12095 = DIRECTION ( 'NONE',  ( 0.000000000000000000, 0.000000000000000000, 1.000000000000000000 ) ) ;
#12096 = COLOUR_RGB ( '', 0.66274510, 0.83137255, 0.94901961) ;
#12097 = CARTESIAN_POINT ( 'NONE',  ( 16.56822296793089322, -0.003834730849371946210, -0.009385634690642043892 ) ) ;
#12098 = CARTESIAN_POINT ( 'NONE',  ( 0.3137051932979792457, -11.37800749014136592, 7.698472063774431717 ) ) ;
#12099 = CARTESIAN_POINT ( 'NONE',  ( 0.3142011359265305392, 8.382042760265909109, 10.88514493056445076 ) ) ;
#12100 = CARTESIAN_POINT ( 'NONE',  ( 0.4384471787762828088, -12.93784327393176881, 4.978024343488995918 ) ) ;
#12101 = B_SPLINE_CURVE_WITH_KNOTS ( 'NONE', 3,
 ( #1711, #286, #6115, #16444, #18412, #16990 ),
 .UNSPECIFIED., .F., .F.,
 ( 4, 2, 4 ),
 ( 9.263427422397552964E-19, 0.001500839035891551789, 0.003001678071783102711 ),
 .UNSPECIFIED. ) ;
#12102 = EDGE_CURVE ( 'NONE', #14389, #7527, #8650, .T. ) ;
#12103 = CARTESIAN_POINT ( 'NONE',  ( 8.522092701127531811, 6.489356537178224471, -2.505958102592553693 ) ) ;
#12104 = CARTESIAN_POINT ( 'NONE',  ( 0.4754618798421162973, 11.68486377711977475, -7.564402563418339831 ) ) ;
#12105 = EDGE_LOOP ( 'NONE', ( #14049, #15733, #16643, #15080 ) ) ;
#12106 = VERTEX_POINT ( 'NONE', #6170 ) ;
#12107 = ORIENTED_EDGE ( 'NONE', *, *, #18338, .T. ) ;
#12108 = AXIS2_PLACEMENT_3D ( 'NONE', #14373, #12843, #11520 ) ;
#12109 = ORIENTED_EDGE ( 'NONE', *, *, #17014, .T. ) ;
#12110 = B_SPLINE_CURVE_WITH_KNOTS ( 'NONE', 3,
 ( #6668, #564, #6389, #12392, #15263, #12219 ),
 .UNSPECIFIED., .F., .F.,
 ( 4, 2, 4 ),
 ( 1.748223473168675632E-18, 0.0002017457492448079337, 0.0004034914984896141327 ),
 .UNSPECIFIED. ) ;
#12111 = CARTESIAN_POINT ( 'NONE',  ( 3.353306896162455253, -3.007732942432324474, -13.62210141459498303 ) ) ;
#12112 = DIRECTION ( 'NONE',  ( 1.000000000000000000, 1.239088197126290570E-16, -0.000000000000000000 ) ) ;
#12113 = DIRECTION ( 'NONE',  ( 5.782411586589358625E-16, -1.000000000000000000, 0.000000000000000000 ) ) ;
#12114 = DIRECTION ( 'NONE',  ( 0.9034263296138832500, 0.000000000000000000, 0.4287433579198481337 ) ) ;
#12115 = CARTESIAN_POINT ( 'NONE',  ( 3.512766787570702043, -7.127386085302744867, -13.25664064834487021 ) ) ;
#12116 = ADVANCED_FACE ( 'NONE', ( #14571 ), #10801, .T. ) ;
#12117 = UNCERTAINTY_MEASURE_WITH_UNIT (LENGTH_MEASURE( 1.000000000000000082E-05 ), #10598, 'distance_accuracy_value', 'NONE');
#12118 = CIRCLE ( 'NONE', #6005, 5.000000000000000888 ) ;
#12119 = ORIENTED_EDGE ( 'NONE', *, *, #3339, .F. ) ;
#12120 = LINE ( 'NONE', #15068, #11891 ) ;
#12121 = FACE_OUTER_BOUND ( 'NONE', #10211, .T. ) ;
#12122 = CARTESIAN_POINT ( 'NONE',  ( 0.4862570985993235340, -0.7479633556561480212, -13.89016912371018186 ) ) ;
#12123 = AXIS2_PLACEMENT_3D ( 'NONE', #5433, #12600, #11005 ) ;
#12124 = CARTESIAN_POINT ( 'NONE',  ( 1.847372867223026738, 0.1054171785008226614, -12.44269075185938433 ) ) ;
#12125 = CARTESIAN_POINT ( 'NONE',  ( 1.977228804421385044, 15.04020501276069588, 3.321884655132254505 ) ) ;
#12126 = CARTESIAN_POINT ( 'NONE',  ( 0.3170788640506441158, 0.1533108587036162707, 13.74111462631963576 ) ) ;
#12127 = AXIS2_PLACEMENT_3D ( 'NONE', #11478, #10495, #4218 ) ;
#12128 = CARTESIAN_POINT ( 'NONE',  ( 2.697797270744668019, 11.26906156738836984, -7.053988368581739721 ) ) ;
#12129 = VECTOR ( 'NONE', #3480, 1000.000000000000000 ) ;
#12130 = VERTEX_POINT ( 'NONE', #14956 ) ;
#12131 = VERTEX_POINT ( 'NONE', #13428 ) ;
#12132 = ORIENTED_EDGE ( 'NONE', *, *, #15343, .F. ) ;
#12133 = VECTOR ( 'NONE', #3561, 1000.000000000000000 ) ;
#12134 = EDGE_LOOP ( 'NONE', ( #17678, #13727, #5184, #15205 ) ) ;
#12135 = CARTESIAN_POINT ( 'NONE',  ( 1.846524061778019421, -7.023652644192194927, -10.27028962889604813 ) ) ;
#12136 = VECTOR ( 'NONE', #16004, 1000.000000000000114 ) ;
#12137 = CONICAL_SURFACE ( 'NONE', #14558, 14.54644660717763927, 0.8559913436420816257 ) ;
#12138 = SPHERICAL_SURFACE ( 'NONE', #10213, 5.000000000000000000 ) ;
#12139 = DIRECTION ( 'NONE',  ( -0.000000000000000000, -0.000000000000000000, -1.000000000000000000 ) ) ;
#12140 = CARTESIAN_POINT ( 'NONE',  ( 3.686287386450715076E-15, -16.60000000000000142, 25.01316734529526187 ) ) ;
#12141 = FACE_OUTER_BOUND ( 'NONE', #282, .T. ) ;
#12142 = ORIENTED_EDGE ( 'NONE', *, *, #1914, .T. ) ;
#12143 = CARTESIAN_POINT ( 'NONE',  ( 5.027901255400304414, 7.499999999999997335, -16.81159201184367902 ) ) ;
#12144 = ADVANCED_FACE ( 'NONE', ( #1490 ), #9081, .F. ) ;
#12145 = CARTESIAN_POINT ( 'NONE',  ( 0.3058872367615226295, -3.664492643742672584, -13.24582953854928569 ) ) ;
#12146 = CARTESIAN_POINT ( 'NONE',  ( -4.479409541426045749, 7.499999999999999112, -16.64412940056556067 ) ) ;
#12147 = CARTESIAN_POINT ( 'NONE',  ( 2.123976203522053741, 7.899625852120402136, -13.47898556379304580 ) ) ;
#12148 = CARTESIAN_POINT ( 'NONE',  ( 0.4754618798421167414, 13.89949764182682657, 0.7484603771384882309 ) ) ;
#12149 = ADVANCED_FACE ( 'NONE', ( #7327 ), #3825, .F. ) ;
#12150 = FACE_OUTER_BOUND ( 'NONE', #6012, .T. ) ;
#12151 = CARTESIAN_POINT ( 'NONE',  ( 0.3137051932979792457, 0.4596302728641686874, -13.73004976592201487 ) ) ;
#12152 = ORIENTED_EDGE ( 'NONE', *, *, #4338, .F. ) ;
#12153 = DIRECTION ( 'NONE',  ( 0.000000000000000000, 0.000000000000000000, 1.000000000000000000 ) ) ;
#12155 = VERTEX_POINT ( 'NONE', #10176 ) ;
#12154 = CARTESIAN_POINT ( 'NONE',  ( 1.846138399168762101, 11.69739621335927815, -4.238866729160283064 ) ) ;
#12156 = DIRECTION ( 'NONE',  ( 0.000000000000000000, 0.000000000000000000, -1.000000000000000000 ) ) ;
#12157 = CARTESIAN_POINT ( 'NONE',  ( 0.3720661004400037664, 11.58636699658225844, -7.524064345033335321 ) ) ;
#12158 = AXIS2_PLACEMENT_3D ( 'NONE', #7908, #13717, #632 ) ;
#12159 = EDGE_LOOP ( 'NONE', ( #18815, #3470, #10660, #15269 ) ) ;
#12160 = CARTESIAN_POINT ( 'NONE',  ( 15.00000000000000711, -24.99999999999999645, 3.000000000000000000 ) ) ;
#12161 = CARTESIAN_POINT ( 'NONE',  ( 0.1174197124922954222, -7.500000000000000888, -14.18273494860523520 ) ) ;
#12162 = VERTEX_POINT ( 'NONE', #12002 ) ;
#12163 = CARTESIAN_POINT ( 'NONE',  ( 1.342453679581834924, 7.902645620902629453, -12.51077660954457293 ) ) ;
#12164 = EDGE_CURVE ( 'NONE', #14694, #5775, #12407, .T. ) ;
#12165 = LINE ( 'NONE', #4899, #3329 ) ;
#12166 = CARTESIAN_POINT ( 'NONE',  ( 0.3170788640506441158, 11.20690911610903839, 7.952793437297615675 ) ) ;
#12167 = CARTESIAN_POINT ( 'NONE',  ( 2.636624412715137922, -6.973567714907947135, 14.46769361191283920 ) ) ;
#12168 = ORIENTED_EDGE ( 'NONE', *, *, #4123, .F. ) ;
#12169 = SURFACE_STYLE_FILL_AREA ( #14928 ) ;
#12170 = CARTESIAN_POINT ( 'NONE',  ( 20.00000000000000000, 2.499999999999998668, -17.00000000000000000 ) ) ;
#12171 = CARTESIAN_POINT ( 'NONE',  ( 2.002547531651519996, -10.57595306287296921, 6.845637710436153434 ) ) ;
#12173 = ORIENTED_EDGE ( 'NONE', *, *, #13093, .T. ) ;
#12172 = LINE ( 'NONE', #12443, #1741 ) ;
#12174 = CARTESIAN_POINT ( 'NONE',  ( 1.560000000000000053, 0.000000000000000000, 0.000000000000000000 ) ) ;
#12175 = B_SPLINE_CURVE_WITH_KNOTS ( 'NONE', 3,
 ( #9824, #9653, #1231, #6881, #15657, #3919, #12517, #2555, #11467, #12886, #14235, #3824, #12796 ),
 .UNSPECIFIED., .F., .F.,
 ( 4, 3, 3, 3, 4 ),
 ( 1.788933584601082316E-18, 0.0002299804304191483382, 0.0004599608082120253344, 0.0006467586077648016917, 0.0008336169836825988323 ),
 .UNSPECIFIED. ) ;
#12176 = ORIENTED_EDGE ( 'NONE', *, *, #14937, .T. ) ;
#12177 = CARTESIAN_POINT ( 'NONE',  ( 3.950837973638677170, 13.10350451991849141, -6.316429227969337923 ) ) ;
#12178 = CARTESIAN_POINT ( 'NONE',  ( 2.320520222536477384, 7.743191299717406828, 13.71278186123164922 ) ) ;
#12179 = B_SPLINE_CURVE_WITH_KNOTS ( 'NONE', 3,
 ( #3315, #1900, #8865, #10396, #10599, #3213, #4475, #10305, #7736, #5893, #2920, #16133, #11738 ),
 .UNSPECIFIED., .F., .F.,
 ( 4, 3, 3, 3, 4 ),
 ( 0.000000000000000000, 0.0002299804304191501543, 0.0004599608082120262018, 0.0006467586077648019086, 0.0008336169836825998080 ),
 .UNSPECIFIED. ) ;
#12180 = ORIENTED_EDGE ( 'NONE', *, *, #15026, .T. ) ;
#12181 = ORIENTED_EDGE ( 'NONE', *, *, #489, .T. ) ;
#12182 = CARTESIAN_POINT ( 'NONE',  ( -205.0000000000000000, -5.000000000000024869, -153.7432847437423789 ) ) ;
#12183 = ORIENTED_EDGE ( 'NONE', *, *, #5050, .T. ) ;
#12184 = DIRECTION ( 'NONE',  ( 1.734723475976806848E-16, -1.000000000000000000, 0.000000000000000000 ) ) ;
#12185 = ORIENTED_EDGE ( 'NONE', *, *, #15126, .F. ) ;
#12186 = EDGE_CURVE ( 'NONE', #17865, #11815, #1943, .T. ) ;
#12187 = EDGE_CURVE ( 'NONE', #14893, #14747, #6495, .T. ) ;
#12188 = ADVANCED_FACE ( 'NONE', ( #6556 ), #17654, .F. ) ;
#12189 = B_SPLINE_CURVE_WITH_KNOTS ( 'NONE', 3,
 ( #15215, #7967, #311, #13775 ),
 .UNSPECIFIED., .F., .F.,
 ( 4, 4 ),
 ( 2.211347213673310975E-17, 0.003005512676784851799 ),
 .UNSPECIFIED. ) ;
#12190 = DIRECTION ( 'NONE',  ( 0.000000000000000000, -1.000000000000000000, 0.000000000000000000 ) ) ;
#12191 = B_SPLINE_CURVE_WITH_KNOTS ( 'NONE', 3,
 ( #13465, #6205, #188, #10706, #17974, #1713 ),
 .UNSPECIFIED., .F., .F.,
 ( 4, 2, 4 ),
 ( 4.206917491929696500E-17, 0.0002014099069817275648, 0.0004028198139634130625 ),
 .UNSPECIFIED. ) ;
#12192 = CARTESIAN_POINT ( 'NONE',  ( 0.8740779401507015045, 14.27348745891557158, -0.8420120399581809689 ) ) ;
#12193 = LINE ( 'NONE', #18199, #13654 ) ;
#12194 = CARTESIAN_POINT ( 'NONE',  ( 0.000000000000000000, 1.805416924949539152E-15, 13.42403576283810906 ) ) ;
#12196 = DIRECTION ( 'NONE',  ( -1.913297951445007622E-16, 1.000000000000000000, 0.000000000000000000 ) ) ;
#12195 =( BOUNDED_SURFACE ( )  B_SPLINE_SURFACE ( 3, 1, ( 
 ( #6208, #11659 ),
 ( #16450, #8977 ),
 ( #8880, #7754 ),
 ( #191, #1619 ) ),
 .UNSPECIFIED., .F., .F., .T. ) 
 B_SPLINE_SURFACE_WITH_KNOTS ( ( 4, 4 ),
 ( 2, 2 ),
 ( 0.000000000000000000, 1.000000000000000000 ),
 ( 0.000000000000000000, 1.000000000000000000 ),
 .UNSPECIFIED. ) 
 GEOMETRIC_REPRESENTATION_ITEM ( )  RATIONAL_B_SPLINE_SURFACE ( (
 ( 1.000000000000000000, 1.000000000000000000),
 ( 0.7792777138730158093, 0.9689936506012928330),
 ( 0.7792777138730158093, 0.9689936506012928330),
 ( 1.000000000000000000, 1.000000000000000000) ) ) 
 REPRESENTATION_ITEM ( '' )  SURFACE ( )  );
#12197 = CARTESIAN_POINT ( 'NONE',  ( 2.123976203522053741, -6.261444813538457943, -14.31368049382976260 ) ) ;
#12198 = CARTESIAN_POINT ( 'NONE',  ( 0.4385251269669950824, 0.7363879510387324467, -13.84299131624728751 ) ) ;
#12199 = CARTESIAN_POINT ( 'NONE',  ( 0.3720661004400040439, -8.694226082900513575, -10.73619472937711983 ) ) ;
#12200 = CARTESIAN_POINT ( 'NONE',  ( 0.3137051932979757485, 7.698472063774634222, -11.37800749014122736 ) ) ;
#12201 = LINE ( 'NONE', #3289, #3877 ) ;
#12202 = CARTESIAN_POINT ( 'NONE',  ( 2.747332970342022840, -14.49942876448586482, -7.555624153089806505 ) ) ;
#12203 = VECTOR ( 'NONE', #5837, 1000.000000000000114 ) ;
#12204 = ORIENTED_EDGE ( 'NONE', *, *, #5498, .T. ) ;
#12205 = ORIENTED_EDGE ( 'NONE', *, *, #17769, .F. ) ;
#12206 = EDGE_LOOP ( 'NONE', ( #14600, #14822, #16135, #11438, #7964 ) ) ;
#12207 = ORIENTED_EDGE ( 'NONE', *, *, #8715, .T. ) ;
#12208 = AXIS2_PLACEMENT_3D ( 'NONE', #1596, #10391, #14685 ) ;
#12209 = CARTESIAN_POINT ( 'NONE',  ( 0.3308579732647025651, -13.74211098745268522, -0.5950689966505779971 ) ) ;
#12210 = LINE ( 'NONE', #10385, #16969 ) ;
#12211 = DIRECTION ( 'NONE',  ( -1.000000000000000000, 6.938893903907227392E-16, 0.000000000000000000 ) ) ;
#12212 = CARTESIAN_POINT ( 'NONE',  ( 8.438534575730034959, 1.899950616255281055, -6.598402093327859319 ) ) ;
#12213 = EDGE_CURVE ( 'NONE', #12695, #2120, #15052, .T. ) ;
#12214 = ORIENTED_EDGE ( 'NONE', *, *, #11134, .T. ) ;
#12215 = CARTESIAN_POINT ( 'NONE',  ( 16.58200780006414732, -0.004047297414158971054, 0.01041078477704053193 ) ) ;
#12216 = CARTESIAN_POINT ( 'NONE',  ( 1.847412631396502025, -11.84727953344286533, 3.804043368582616935 ) ) ;
#12217 = EDGE_CURVE ( 'NONE', #5916, #13259, #10489, .T. ) ;
#12218 = CARTESIAN_POINT ( 'NONE',  ( 8.438534575730034959, 5.688336279099100778, -3.845978796785973763 ) ) ;
#12219 = CARTESIAN_POINT ( 'NONE',  ( 0.4862570985993235340, 12.97920246947886191, -5.003653737315353567 ) ) ;
#12220 = DIRECTION ( 'NONE',  ( 0.000000000000000000, 0.000000000000000000, 1.000000000000000000 ) ) ;
#12221 = CARTESIAN_POINT ( 'NONE',  ( 2.636624412714237309, 15.91454522070173638, -2.161493821596664144 ) ) ;
#12222 = EDGE_CURVE ( 'NONE', #4080, #11214, #11706, .T. ) ;
#12223 = ORIENTED_EDGE ( 'NONE', *, *, #13469, .T. ) ;
#12224 = EDGE_LOOP ( 'NONE', ( #5348, #3269, #17040, #14105 ) ) ;
#12225 = EDGE_LOOP ( 'NONE', ( #15746, #8677, #13398, #2011 ) ) ;
#12226 = ORIENTED_EDGE ( 'NONE', *, *, #14106, .T. ) ;
#12227 = CARTESIAN_POINT ( 'NONE',  ( 0.8740779401512879243, 13.31469722824398794, -5.211551231203936929 ) ) ;
#12228 = CARTESIAN_POINT ( 'NONE',  ( 0.4862570985993235340, 3.580942890621860109, -13.44146924561377254 ) ) ;
#12229 = CARTESIAN_POINT ( 'NONE',  ( 1.846955891736113298, -7.525208385419886348, -9.909315188408124087 ) ) ;
#12230 = PRODUCT_RELATED_PRODUCT_CATEGORY ( 'part', '', ( #1414 ) ) ;
#12231 = CARTESIAN_POINT ( 'NONE',  ( 16.57778382496167424, 0.002851818597093403688, 0.01466529584256672306 ) ) ;
#12232 = EDGE_CURVE ( 'NONE', #6002, #3979, #17668, .T. ) ;
#12233 = DIRECTION ( 'NONE',  ( 0.000000000000000000, 0.000000000000000000, 1.000000000000000000 ) ) ;
#12234 = VERTEX_POINT ( 'NONE', #8083 ) ;
#12235 = CARTESIAN_POINT ( 'NONE',  ( -1.149044392847440088, 7.500000000000000000, -14.62466132081332582 ) ) ;
#12236 = CARTESIAN_POINT ( 'NONE',  ( 0.3145729642390426295, 13.15786090015083687, 3.952965287571154729 ) ) ;
#12237 = EDGE_CURVE ( 'NONE', #17311, #4902, #8293, .T. ) ;
#12238 = ADVANCED_FACE ( 'NONE', ( #12376 ), #1884, .F. ) ;
#12239 = CARTESIAN_POINT ( 'NONE',  ( -0.9490252293515478721, 6.938433416811056631, -12.00000000290481239 ) ) ;
#12240 = CARTESIAN_POINT ( 'NONE',  ( 16.56782317627811096, -0.009439921864426449247, -0.002708056627497712563 ) ) ;
#12241 = DIRECTION ( 'NONE',  ( 0.000000000000000000, 0.000000000000000000, -1.000000000000000000 ) ) ;
#12242 = CARTESIAN_POINT ( 'NONE',  ( 3.950837973638676281, 14.31366178983253512, 2.591948120961855118 ) ) ;
#12243 = FACE_OUTER_BOUND ( 'NONE', #18101, .T. ) ;
#12244 = ORIENTED_EDGE ( 'NONE', *, *, #18401, .F. ) ;
#12246 = ORIENTED_EDGE ( 'NONE', *, *, #6516, .T. ) ;
#12245 = DIRECTION ( 'NONE',  ( -1.000000000000000000, -0.000000000000000000, -0.000000000000000000 ) ) ;
#12247 = CARTESIAN_POINT ( 'NONE',  ( -4.999999999999995559, -27.00000000000000000, 31.00000000000000000 ) ) ;
#12248 = EDGE_CURVE ( 'NONE', #8289, #11928, #6819, .T. ) ;
#12249 = EDGE_LOOP ( 'NONE', ( #15824, #2026, #4821 ) ) ;
#12250 = CARTESIAN_POINT ( 'NONE',  ( 0.3095370825347224519, -12.91933430393604709, -4.681152801286295073 ) ) ;
#12251 = CARTESIAN_POINT ( 'NONE',  ( -0.3159797039860490209, -6.996005774985150083, -11.99999999647927496 ) ) ;
#12252 = VERTEX_POINT ( 'NONE', #18384 ) ;
#12253 = CARTESIAN_POINT ( 'NONE',  ( 12.00000000000000711, -14.99999999999999645, 7.000000000000000000 ) ) ;
#12254 = CARTESIAN_POINT ( 'NONE',  ( 2.002547531651519996, 4.532360870844327039, 11.75462648437103752 ) ) ;
#12255 = CARTESIAN_POINT ( 'NONE',  ( 1.977228804422059394, -15.33060379559095310, 1.488378900182341091 ) ) ;
#12256 = PLANE ( 'NONE',  #17883 ) ;
#12257 = CIRCLE ( 'NONE', #16536, 12.00000000000000178 ) ;
#12258 = CARTESIAN_POINT ( 'NONE',  ( 0.3151928479966097374, 0.000000000000000000, -13.73922861026898623 ) ) ;
#12259 =( BOUNDED_SURFACE ( )  B_SPLINE_SURFACE ( 3, 1, ( 
 ( #154, #8934 ),
 ( #1677, #252 ),
 ( #11908, #17745 ),
 ( #4647, #10472 ) ),
 .UNSPECIFIED., .F., .F., .T. ) 
 B_SPLINE_SURFACE_WITH_KNOTS ( ( 4, 4 ),
 ( 2, 2 ),
 ( 0.000000000000000000, 1.000000000000000000 ),
 ( 0.000000000000000000, 1.000000000000000000 ),
 .UNSPECIFIED. ) 
 GEOMETRIC_REPRESENTATION_ITEM ( )  RATIONAL_B_SPLINE_SURFACE ( (
 ( 1.000000000000000000, 1.000000000000000000),
 ( 0.9933953342250436691, 0.8357391271907733676),
 ( 0.9933953342250436691, 0.8357391271907733676),
 ( 1.000000000000000000, 1.000000000000000000) ) ) 
 REPRESENTATION_ITEM ( '' )  SURFACE ( )  );
#12260 = DIRECTION ( 'NONE',  ( 0.000000000000000000, 0.000000000000000000, 1.000000000000000000 ) ) ;
#12262 = ORIENTED_EDGE ( 'NONE', *, *, #10347, .F. ) ;
#12261 = CARTESIAN_POINT ( 'NONE',  ( 0.000000000000000000, 0.000000000000000000, 5.000000000000000000 ) ) ;
#12263 = CARTESIAN_POINT ( 'NONE',  ( 0.4862570985993235340, 8.769551628660890330, -10.79774104611363761 ) ) ;
#12264 = EDGE_CURVE ( 'NONE', #14938, #14465, #9886, .T. ) ;
#12265 = EDGE_LOOP ( 'NONE', ( #12246, #16113 ) ) ;
#12266 = CARTESIAN_POINT ( 'NONE',  ( 1.959283090834842200, -11.71721539537258394, 4.509128209890929107 ) ) ;
#12267 = ORIENTED_EDGE ( 'NONE', *, *, #560, .F. ) ;
#12268 = ORIENTED_EDGE ( 'NONE', *, *, #3271, .F. ) ;
#12269 = CARTESIAN_POINT ( 'NONE',  ( 0.3148208552358927048, 10.97826876274324270, -8.260375059853219071 ) ) ;
#12270 = EDGE_LOOP ( 'NONE', ( #11789, #8560, #2266, #13793 ) ) ;
#12271 = CARTESIAN_POINT ( 'NONE',  ( 15.00000000000000711, -14.99999999999999645, 8.000000000000000000 ) ) ;
#12272 = ORIENTED_EDGE ( 'NONE', *, *, #10849, .F. ) ;
#12273 = CARTESIAN_POINT ( 'NONE',  ( 2.636624412715137922, 2.161493821597615828, 15.91454522070216093 ) ) ;
#12274 = FACE_BOUND ( 'NONE', #2676, .T. ) ;
#12275 = CIRCLE ( 'NONE', #6175, 14.54644660717763927 ) ;
#12276 = FACE_OUTER_BOUND ( 'NONE', #10818, .T. ) ;
#12277 = CARTESIAN_POINT ( 'NONE',  ( 0.3308579732647022875, 13.25341063505880967, -3.680601586799737923 ) ) ;
#12278 = PRODUCT ( 'Handle arm 2', 'Handle arm 2', '', ( #3671 ) ) ;
#12279 = CARTESIAN_POINT ( 'NONE',  ( 2.123976203522053297, 6.261444813538757259, -14.31368049382962937 ) ) ;
#12280 = PRODUCT_CONTEXT ( 'NONE', #8629, 'mechanical' ) ;
#12281 = DIRECTION ( 'NONE',  ( -1.000000000000000000, 0.000000000000000000, 0.000000000000000000 ) ) ;
#12282 = CARTESIAN_POINT ( 'NONE',  ( 0.3150686449036038117, 8.199336701264542171, 11.02450593298021175 ) ) ;
#12283 = DIRECTION ( 'NONE',  ( -0.000000000000000000, -0.000000000000000000, 1.000000000000000000 ) ) ;
#12284 = ADVANCED_FACE ( 'NONE', ( #6744 ), #9772, .F. ) ;
#12285 = EDGE_CURVE ( 'NONE', #17303, #4602, #12616, .T. ) ;
#12286 = EDGE_CURVE ( 'NONE', #3873, #14201, #14359, .T. ) ;
#12287 = SPHERICAL_SURFACE ( 'NONE', #17619, 5.000000000000000000 ) ;
#12288 = VERTEX_POINT ( 'NONE', #5649 ) ;
#12289 = ORIENTED_EDGE ( 'NONE', *, *, #3537, .T. ) ;
#12290 = VERTEX_POINT ( 'NONE', #3957 ) ;
#12291 = ORIENTED_EDGE ( 'NONE', *, *, #1658, .F. ) ;
#12292 = ORIENTED_EDGE ( 'NONE', *, *, #11206, .T. ) ;
#12293 = B_SPLINE_CURVE_WITH_KNOTS ( 'NONE', 3,
 ( #10484, #6092, #7727, #13536 ),
 .UNSPECIFIED., .F., .F.,
 ( 4, 4 ),
 ( 1.182319362138779820E-16, 0.002004993803842621859 ),
 .UNSPECIFIED. ) ;
#12294 =( BOUNDED_SURFACE ( )  B_SPLINE_SURFACE ( 3, 1, ( 
 ( #8194, #18313 ),
 ( #918, #18043 ),
 ( #4857, #6759 ),
 ( #649, #7926 ) ),
 .UNSPECIFIED., .F., .F., .T. ) 
 B_SPLINE_SURFACE_WITH_KNOTS ( ( 4, 4 ),
 ( 2, 2 ),
 ( 0.000000000000000000, 1.000000000000000000 ),
 ( 0.000000000000000000, 1.000000000000000000 ),
 .UNSPECIFIED. ) 
 GEOMETRIC_REPRESENTATION_ITEM ( )  RATIONAL_B_SPLINE_SURFACE ( (
 ( 1.000000000000000000, 1.000000000000000000),
 ( 0.7792777138730158093, 0.9689936506012928330),
 ( 0.7792777138730158093, 0.9689936506012928330),
 ( 1.000000000000000000, 1.000000000000000000) ) ) 
 REPRESENTATION_ITEM ( '' )  SURFACE ( )  );
#12295 =( BOUNDED_SURFACE ( )  B_SPLINE_SURFACE ( 3, 1, ( 
 ( #18324, #16718 ),
 ( #3617, #9451 ),
 ( #12494, #9720 ),
 ( #5231, #15275 ) ),
 .UNSPECIFIED., .F., .F., .T. ) 
 B_SPLINE_SURFACE_WITH_KNOTS ( ( 4, 4 ),
 ( 2, 2 ),
 ( 0.000000000000000000, 1.000000000000000000 ),
 ( 0.000000000000000000, 1.000000000000000000 ),
 .UNSPECIFIED. ) 
 GEOMETRIC_REPRESENTATION_ITEM ( )  RATIONAL_B_SPLINE_SURFACE ( (
 ( 1.000000000000000000, 1.000000000000000000),
 ( 0.7792777138730160313, 0.9689936506012927220),
 ( 0.7792777138730160313, 0.9689936506012927220),
 ( 1.000000000000000000, 1.000000000000000000) ) ) 
 REPRESENTATION_ITEM ( '' )  SURFACE ( )  );
#12296 = CARTESIAN_POINT ( 'NONE',  ( 0.3939875929385628361, 12.90850834464107244, -4.930599594904421679 ) ) ;
#12297 = EDGE_CURVE ( 'NONE', #7502, #10742, #12554, .T. ) ;
#12298 = CARTESIAN_POINT ( 'NONE',  ( 0.3137051932979792457, 4.679953077377670745, -12.91601973349265720 ) ) ;
#12299 = ORIENTED_EDGE ( 'NONE', *, *, #18832, .F. ) ;
#12300 = DIRECTION ( 'NONE',  ( 1.000000000000000000, -0.000000000000000000, -0.000000000000000000 ) ) ;
#12301 = CARTESIAN_POINT ( 'NONE',  ( 8.522092701127531811, 3.777034505568523048, 5.841710761610143798 ) ) ;
#12302 = CARTESIAN_POINT ( 'NONE',  ( 16.57778382496167424, 0.01354073047775767452, 0.006312874906843726416 ) ) ;
#12303 = DIRECTION ( 'NONE',  ( 0.000000000000000000, 0.000000000000000000, 1.000000000000000000 ) ) ;
#12304 = CARTESIAN_POINT ( 'NONE',  ( 2.705023505549862151, 8.489131503859777439, 10.24007717649583782 ) ) ;
#12305 = DIRECTION ( 'NONE',  ( -0.7561779333270775005, -0.2350349629540143537, -0.6106991889125079620 ) ) ;
#12306 = CONICAL_SURFACE ( 'NONE', #1616, 14.54644660717763927, 0.8559913436420816257 ) ;
#12307 = ORIENTED_EDGE ( 'NONE', *, *, #5123, .F. ) ;
#12308 = EDGE_CURVE ( 'NONE', #15961, #2927, #11048, .T. ) ;
#12309 = EDGE_LOOP ( 'NONE', ( #3418, #2180, #11346, #1761, #14622 ) ) ;
#12310 = VERTEX_POINT ( 'NONE', #18750 ) ;
#12311 = EDGE_CURVE ( 'NONE', #4533, #7061, #10828, .T. ) ;
#12312 = ORIENTED_EDGE ( 'NONE', *, *, #17793, .T. ) ;
#12313 = CARTESIAN_POINT ( 'NONE',  ( 0.4862570985993235340, 12.97920246947886191, -5.003653737315353567 ) ) ;
#12314 = FACE_OUTER_BOUND ( 'NONE', #8365, .T. ) ;
#12315 = CARTESIAN_POINT ( 'NONE',  ( 1.847034903785819360, -7.126331315909195219, -10.19974412751572679 ) ) ;
#12316 = CARTESIAN_POINT ( 'NONE',  ( 14.99999999999999289, 20.00000000000000000, 3.000000000000000000 ) ) ;
#12317 = CARTESIAN_POINT ( 'NONE',  ( 3.074695600507241444, -15.30693405987796751, 2.772091048739207864 ) ) ;
#12318 = ORIENTED_EDGE ( 'NONE', *, *, #12615, .F. ) ;
#12319 = LINE ( 'NONE', #13839, #17864 ) ;
#12320 = EDGE_CURVE ( 'NONE', #3538, #617, #3038, .T. ) ;
#12321 = DIRECTION ( 'NONE',  ( 0.7561779333270775005, 0.6534392409364817578, 0.03481510524965471948 ) ) ;
#12322 = B_SPLINE_CURVE_WITH_KNOTS ( 'NONE', 3,
 ( #2778, #8625, #1361, #4418, #7104, #8905 ),
 .UNSPECIFIED., .F., .F.,
 ( 4, 2, 4 ),
 ( 0.000000000000000000, 0.001500839035891552223, 0.003001678071783104446 ),
 .UNSPECIFIED. ) ;
#12323 = CARTESIAN_POINT ( 'NONE',  ( 0.3159797039863193602, 6.996005774985157188, -11.99999999647930871 ) ) ;
#12324 = CARTESIAN_POINT ( 'NONE',  ( 1.861628059977344263, -6.879051339207215676, -10.38573835516720401 ) ) ;
#12325 = CARTESIAN_POINT ( 'NONE',  ( 16.57778382496167424, -0.002851818597093896349, 0.01466529584256787665 ) ) ;
#12326 = CARTESIAN_POINT ( 'NONE',  ( 0.3142014840576502488, 13.17932813834300099, -3.879477880151306568 ) ) ;
#12327 = VERTEX_POINT ( 'NONE', #17135 ) ;
#12329 = ORIENTED_EDGE ( 'NONE', *, *, #269, .T. ) ;
#12328 = DIRECTION ( 'NONE',  ( 1.000000000000000000, 0.000000000000000000, 0.000000000000000000 ) ) ;
#12330 = DIRECTION ( 'NONE',  ( -1.000000000000000000, -0.000000000000000000, -0.000000000000000000 ) ) ;
#12331 = VECTOR ( 'NONE', #1426, 1000.000000000000114 ) ;
#12332 = CARTESIAN_POINT ( 'NONE',  ( 16.56753206892534891, -0.008490833999798035742, 0.004253784598196731770 ) ) ;
#12333 = ORIENTED_EDGE ( 'NONE', *, *, #12074, .T. ) ;
#12334 = CARTESIAN_POINT ( 'NONE',  ( 0.4754618798421162973, 11.68486377711966817, 7.564402563418513026 ) ) ;
#12335 = CARTESIAN_POINT ( 'NONE',  ( -0.5544330523543454792, -7.500000000000000888, -14.29923508549715194 ) ) ;
#12336 = EDGE_CURVE ( 'NONE', #8092, #1784, #3019, .T. ) ;
#12337 = ORIENTED_EDGE ( 'NONE', *, *, #5415, .F. ) ;
#12338 = LINE ( 'NONE', #6612, #16706 ) ;
#12339 = CARTESIAN_POINT ( 'NONE',  ( -33.49999999999999289, -12.50000000000000178, 6.500000000000000888 ) ) ;
#12340 = DIRECTION ( 'NONE',  ( 0.000000000000000000, 0.000000000000000000, -1.000000000000000000 ) ) ;
#12341 = CARTESIAN_POINT ( 'NONE',  ( 2.426025403784448642, 0.000000000000000000, 2.168404344971008868E-16 ) ) ;
#12342 = EDGE_CURVE ( 'NONE', #622, #16531, #8441, .T. ) ;
#12343 = AXIS2_PLACEMENT_3D ( 'NONE', #11322, #18478, #14454 ) ;
#12344 = PRESENTATION_STYLE_ASSIGNMENT (( #1845 ) ) ;
#12345 = CARTESIAN_POINT ( 'NONE',  ( 1.847372867223027848, -10.12831093686727080, 7.228345833872717563 ) ) ;
#12346 = CARTESIAN_POINT ( 'NONE',  ( 16.56872352241294521, 0.01027347319884366721, 0.001821578298043820656 ) ) ;
#12348 = ORIENTED_EDGE ( 'NONE', *, *, #3114, .F. ) ;
#12347 = LINE ( 'NONE', #5177, #14540 ) ;
#12349 = LINE ( 'NONE', #17911, #1758 ) ;
#12350 = B_SPLINE_CURVE_WITH_KNOTS ( 'NONE', 3,
 ( #9154, #16795, #13823, #739, #6669, #18315 ),
 .UNSPECIFIED., .F., .F.,
 ( 4, 2, 4 ),
 ( 2.462833906345087556E-18, 0.0001828790815886951863, 0.0003657581631773856022 ),
 .UNSPECIFIED. ) ;
#12351 = VERTEX_POINT ( 'NONE', #9962 ) ;
#12352 = CARTESIAN_POINT ( 'NONE',  ( 0.3145734862173208413, -10.93207848441427643, -8.321353293018953323 ) ) ;
#12353 = CARTESIAN_POINT ( 'NONE',  ( -25.00000000000000000, -7.500000000000000888, -17.00000000000000000 ) ) ;
#12354 = ORIENTED_EDGE ( 'NONE', *, *, #2024, .T. ) ;
#12355 = VECTOR ( 'NONE', #6565, 1000.000000000000000 ) ;
#12356 = ORIENTED_EDGE ( 'NONE', *, *, #14050, .F. ) ;
#12357 = DIRECTION ( 'NONE',  ( -1.000000000000000000, 0.000000000000000000, -0.000000000000000000 ) ) ;
#12358 = CARTESIAN_POINT ( 'NONE',  ( 2.636624412714236865, 0.000000000000000000, 0.000000000000000000 ) ) ;
#12359 = AXIS2_PLACEMENT_3D ( 'NONE', #18628, #5622, #14522 ) ;
#12360 = VERTEX_POINT ( 'NONE', #15796 ) ;
#12361 = VECTOR ( 'NONE', #10986, 1000.000000000000114 ) ;
#12362 = ADVANCED_FACE ( 'NONE', ( #12924 ), #5900, .T. ) ;
#12363 = SURFACE_STYLE_FILL_AREA ( #626 ) ;
#12364 = DIRECTION ( 'NONE',  ( -1.000000000000000000, 0.000000000000000000, -0.000000000000000000 ) ) ;
#12365 = CARTESIAN_POINT ( 'NONE',  ( 0.000000000000000000, 0.000000000000000000, -3.000000000000000000 ) ) ;
#12366 = CARTESIAN_POINT ( 'NONE',  ( 18.75000000000000000, 0.000000000000000000, 2.055000000000000160 ) ) ;
#12367 = EDGE_CURVE ( 'NONE', #17792, #14367, #8723, .T. ) ;
#12368 = B_SPLINE_CURVE_WITH_KNOTS ( 'NONE', 3,
 ( #11847, #2936, #1233, #3028, #15757, #7073, #13176 ),
 .UNSPECIFIED., .F., .F.,
 ( 4, 3, 4 ),
 ( 1.951563910473907981E-18, 0.0002299804304191482840, 0.0004168119862248656667 ),
 .UNSPECIFIED. ) ;
#12369 = CARTESIAN_POINT ( 'NONE',  ( 16.56822296793089322, 0.008619100080559776930, 0.005339139727952691740 ) ) ;
#12370 = PRODUCT_CONTEXT ( 'NONE', #12539, 'mechanical' ) ;
#12371 =( BOUNDED_SURFACE ( )  B_SPLINE_SURFACE ( 3, 1, ( 
 ( #14015, #18047 ),
 ( #18317, #17960 ),
 ( #9528, #9444 ),
 ( #16528, #15268 ) ),
 .UNSPECIFIED., .F., .F., .T. ) 
 B_SPLINE_SURFACE_WITH_KNOTS ( ( 4, 4 ),
 ( 2, 2 ),
 ( 0.000000000000000000, 1.000000000000000000 ),
 ( 0.000000000000000000, 1.000000000000000000 ),
 .UNSPECIFIED. ) 
 GEOMETRIC_REPRESENTATION_ITEM ( )  RATIONAL_B_SPLINE_SURFACE ( (
 ( 1.000000000000000000, 1.000000000000000000),
 ( 0.9933953342250438912, 0.8357391271907739227),
 ( 0.9933953342250438912, 0.8357391271907739227),
 ( 1.000000000000000000, 1.000000000000000000) ) ) 
 REPRESENTATION_ITEM ( '' )  SURFACE ( )  );
#12372 = PRESENTATION_STYLE_ASSIGNMENT (( #811 ) ) ;
#12373 = CARTESIAN_POINT ( 'NONE',  ( -110.4113270445337918, -81.60345299795268659, -91.28051051278382033 ) ) ;
#12374 = CARTESIAN_POINT ( 'NONE',  ( 1.918918678667043576, 3.258447776120001915, -12.08296592096904298 ) ) ;
#12375 = VECTOR ( 'NONE', #12522, 1000.000000000000000 ) ;
#12376 = FACE_OUTER_BOUND ( 'NONE', #11646, .T. ) ;
#12377 = DIRECTION ( 'NONE',  ( -0.4246593920385851040, -0.1376957914266804250, 0.8948208031649687033 ) ) ;
#12378 = CARTESIAN_POINT ( 'NONE',  ( 2.636624412715137034, -11.60464335004055947, 11.10302021257951743 ) ) ;
#12379 = LINE ( 'NONE', #18209, #9970 ) ;
#12380 = ORIENTED_EDGE ( 'NONE', *, *, #12807, .F. ) ;
#12381 = ORIENTED_EDGE ( 'NONE', *, *, #7039, .T. ) ;
#12382 = ORIENTED_EDGE ( 'NONE', *, *, #10331, .T. ) ;
#12383 = ORIENTED_EDGE ( 'NONE', *, *, #8315, .F. ) ;
#12384 = ORIENTED_EDGE ( 'NONE', *, *, #6070, .F. ) ;
#12385 = CARTESIAN_POINT ( 'NONE',  ( 1.861706995891668104, -9.751699138048492088, 7.751853334747282886 ) ) ;
#12386 = CARTESIAN_POINT ( 'NONE',  ( 0.4862570985993235340, -10.79774104611366781, -8.769551628660854803 ) ) ;
#12387 = ADVANCED_FACE ( 'NONE', ( #11880 ), #10932, .F. ) ;
#12388 = ORIENTED_EDGE ( 'NONE', *, *, #15101, .F. ) ;
#12389 = CARTESIAN_POINT ( 'NONE',  ( 2.123976203522053297, 7.899625852120206737, 13.47898556379315771 ) ) ;
#12390 = CARTESIAN_POINT ( 'NONE',  ( 1.846138399168762101, -11.95493567637852905, 3.446241763652952539 ) ) ;
#12391 = CARTESIAN_POINT ( 'NONE',  ( 1.846138399168762101, -4.238866729160323032, -11.69739621335926394 ) ) ;
#12392 = CARTESIAN_POINT ( 'NONE',  ( 0.3939875929385628361, 12.90850834464107244, -4.930599594904421679 ) ) ;
#12393 = DIRECTION ( 'NONE',  ( 0.000000000000000000, 0.000000000000000000, 1.000000000000000000 ) ) ;
#12394 = CARTESIAN_POINT ( 'NONE',  ( 1.254009781011619307, -11.25324419414205224, 9.426200207651413976 ) ) ;
#12395 = LINE ( 'NONE', #18230, #6010 ) ;
#12396 = ORIENTED_EDGE ( 'NONE', *, *, #11690, .T. ) ;
#12397 = AXIS2_PLACEMENT_3D ( 'NONE', #10613, #2105, #6496 ) ;
#12398 = PRESENTATION_LAYER_ASSIGNMENT (  '', '', ( #3844 ) ) ;
#12399 = ORIENTED_EDGE ( 'NONE', *, *, #16832, .T. ) ;
#12400 = ORIENTED_EDGE ( 'NONE', *, *, #12232, .T. ) ;
#12401 = VERTEX_POINT ( 'NONE', #15889 ) ;
#12402 =( BOUNDED_SURFACE ( )  B_SPLINE_SURFACE ( 3, 1, ( 
 ( #18246, #14114 ),
 ( #15365, #18415 ),
 ( #2367, #15280 ),
 ( #8124, #5328 ) ),
 .UNSPECIFIED., .F., .F., .T. ) 
 B_SPLINE_SURFACE_WITH_KNOTS ( ( 4, 4 ),
 ( 2, 2 ),
 ( 0.000000000000000000, 1.000000000000000000 ),
 ( 0.000000000000000000, 1.000000000000000000 ),
 .UNSPECIFIED. ) 
 GEOMETRIC_REPRESENTATION_ITEM ( )  RATIONAL_B_SPLINE_SURFACE ( (
 ( 1.000000000000000000, 1.000000000000000000),
 ( 0.9933953342250436691, 0.8357391271907733676),
 ( 0.9933953342250436691, 0.8357391271907733676),
 ( 1.000000000000000000, 1.000000000000000000) ) ) 
 REPRESENTATION_ITEM ( '' )  SURFACE ( )  );
#12403 = LINE ( 'NONE', #10983, #3108 ) ;
#12404 = CARTESIAN_POINT ( 'NONE',  ( 18.30499999999999972, 0.000000000000000000, 2.499999999999999556 ) ) ;
#12405 = CARTESIAN_POINT ( 'NONE',  ( 3.950837973638675393, 14.31366178983257242, -2.591948120961654833 ) ) ;
#12406 = CARTESIAN_POINT ( 'NONE',  ( 16.58200780006414732, -0.01041078477704051979, -0.004047297414159007484 ) ) ;
#12407 = B_SPLINE_CURVE_WITH_KNOTS ( 'NONE', 3,
 ( #17643, #16002, #4549, #4738, #16111, #2894 ),
 .UNSPECIFIED., .F., .F.,
 ( 4, 2, 4 ),
 ( 4.014301552767626103E-17, 0.0002014099069817288116, 0.0004028198139634175078 ),
 .UNSPECIFIED. ) ;
#12408 = CARTESIAN_POINT ( 'NONE',  ( -5.000000000000000000, 20.00000000000000000, 8.000000000000000000 ) ) ;
#12409 = ORIENTED_EDGE ( 'NONE', *, *, #15117, .T. ) ;
#12410 = EDGE_CURVE ( 'NONE', #5432, #16388, #3473, .T. ) ;
#12411 = CARTESIAN_POINT ( 'NONE',  ( 6.538348415311010520, 7.499999999999999112, -16.99999999999999645 ) ) ;
#12412 = EDGE_CURVE ( 'NONE', #473, #8092, #13297, .T. ) ;
#12413 = AXIS2_PLACEMENT_3D ( 'NONE', #394, #14914, #1930 ) ;
#12414 = CARTESIAN_POINT ( 'NONE',  ( 16.57210152137263393, -0.0006600038696348781500, -0.01453130299868639688 ) ) ;
#12415 = ADVANCED_FACE ( 'NONE', ( #122 ), #7121, .F. ) ;
#12416 = CARTESIAN_POINT ( 'NONE',  ( 0.7340363079801778268, 6.964562493341673211, -12.00000000352069307 ) ) ;
#12417 = CARTESIAN_POINT ( 'NONE',  ( 1.254255976358044311, -7.789651112956927470, -12.44256109021856105 ) ) ;
#12418 = STYLED_ITEM ( 'NONE', ( #11317 ), #16761 ) ;
#12419 = VECTOR ( 'NONE', #5643, 1000.000000000000000 ) ;
#12420 = CARTESIAN_POINT ( 'NONE',  ( 0.3095370825347233956, 3.806662003783596759, -13.20347358821910433 ) ) ;
#12421 = DIRECTION ( 'NONE',  ( -1.000000000000000000, -0.000000000000000000, -0.000000000000000000 ) ) ;
#12422 = CARTESIAN_POINT ( 'NONE',  ( 3.377929128793397684, -9.234024516648242198, -10.50432311212913028 ) ) ;
#12423 = CARTESIAN_POINT ( 'NONE',  ( 1.254255976357895763, -3.563435620217493494, -14.24071337840814166 ) ) ;
#12424 = EDGE_LOOP ( 'NONE', ( #8299, #6380, #3357, #2267 ) ) ;
#12425 = AXIS2_PLACEMENT_3D ( 'NONE', #18830, #8335, #15581 ) ;
#12427 = ORIENTED_EDGE ( 'NONE', *, *, #13250, .T. ) ;
#12426 = CARTESIAN_POINT ( 'NONE',  ( 5.000000000000000888, 17.00000000000000000, 7.000000000000000000 ) ) ;
#12428 = CARTESIAN_POINT ( 'NONE',  ( 2.123976203522053297, -14.31368049382965069, -6.261444813538707521 ) ) ;
#12429 = AXIS2_PLACEMENT_3D ( 'NONE', #18479, #18658, #9861 ) ;
#12430 = CLOSED_SHELL ( 'NONE', ( #10477, #18464, #2802, #7988, #12612, #1660, #7326, #4074, #5239, #13336, #18009, #5511, #7201, #5779, #2204, #18531, #13703, #12512, #1224, #7284, #9758, #11691, #2569, #15362, #18289, #3727, #2112, #13035, #2130, #3097, #9465, #16503, #8566, #10000, #15427 ) ) ;
#12431 = ORIENTED_EDGE ( 'NONE', *, *, #513, .T. ) ;
#12432 = CARTESIAN_POINT ( 'NONE',  ( 1.861706995891666550, -4.359009869687166194, -11.66987142852988946 ) ) ;
#12433 = CARTESIAN_POINT ( 'NONE',  ( -5.763005853485871910, -3.979914285031270538, -11.99999999870361655 ) ) ;
#12434 = ORIENTED_EDGE ( 'NONE', *, *, #15204, .T. ) ;
#12435 = CARTESIAN_POINT ( 'NONE',  ( 1.847168016377985333, -7.161712042621529939, 10.17509564929255994 ) ) ;
#12436 = CARTESIAN_POINT ( 'NONE',  ( 2.636624412716062071, -14.14563173255412742, -7.605649742760987486 ) ) ;
#12437 = CARTESIAN_POINT ( 'NONE',  ( 3.512766787570921867, 14.81029789862138912, 2.682019731918403593 ) ) ;
#12438 = DIRECTION ( 'NONE',  ( 0.000000000000000000, -0.000000000000000000, -1.000000000000000000 ) ) ;
#12439 = CIRCLE ( 'NONE', #2946, 3.499999999999992895 ) ;
#12440 = ADVANCED_FACE ( 'NONE', ( #24 ), #12856, .F. ) ;
#12441 = CARTESIAN_POINT ( 'NONE',  ( 16.57210152137263393, 0.008007331252332874558, 0.01214401161737521141 ) ) ;
#12442 = CARTESIAN_POINT ( 'NONE',  ( 0.3058872367615230181, 0.6080468242580958638, 13.72992299905060243 ) ) ;
#12444 = ORIENTED_EDGE ( 'NONE', *, *, #2888, .T. ) ;
#12443 = CARTESIAN_POINT ( 'NONE',  ( 8.522092701127531811, 0.3779863304871219909, 6.946128462138597470 ) ) ;
#12445 = CARTESIAN_POINT ( 'NONE',  ( 16.57210152137263393, -0.01214401161737523396, 0.008007331252332839863 ) ) ;
#12446 = B_SPLINE_CURVE_WITH_KNOTS ( 'NONE', 3,
 ( #10562, #11898, #17529, #16398, #7510, #17927 ),
 .UNSPECIFIED., .F., .F.,
 ( 4, 2, 4 ),
 ( 4.023840028577795923E-17, 0.0002014099069817275377, 0.0004028198139634147973 ),
 .UNSPECIFIED. ) ;
#12447 = ORIENTED_EDGE ( 'NONE', *, *, #13767, .F. ) ;
#12448 = LINE ( 'NONE', #12532, #12133 ) ;
#12449 = CARTESIAN_POINT ( 'NONE',  ( 1.846138399168762101, 11.69739621335927815, -4.238866729160283064 ) ) ;
#12450 = EDGE_LOOP ( 'NONE', ( #11685, #4202, #17917, #1999 ) ) ;
#12451 = ORIENTED_EDGE ( 'NONE', *, *, #10626, .F. ) ;
#12452 = CARTESIAN_POINT ( 'NONE',  ( 2.636624412715362631, -15.80357026013197519, 2.862162146984090327 ) ) ;
#12453 = CARTESIAN_POINT ( 'NONE',  ( 3.512766787570877902, 13.25664064834461264, 7.127386085302796381 ) ) ;
#12454 = ORIENTED_EDGE ( 'NONE', *, *, #7200, .F. ) ;
#12455 = CARTESIAN_POINT ( 'NONE',  ( 16.58200780006414732, -0.009393638146078483672, -0.006043560077721808060 ) ) ;
#12456 = CARTESIAN_POINT ( 'NONE',  ( 0.8740779401510752056, 3.609949156401575543, -13.83508928787453662 ) ) ;
#12457 = CARTESIAN_POINT ( 'NONE',  ( 16.56872352241294521, 0.001442253899401802278, 0.01033355228142402403 ) ) ;
#12458 = ADVANCED_FACE ( 'NONE', ( #8626 ), #4594, .F. ) ;
#12459 = CARTESIAN_POINT ( 'NONE',  ( 6.071532165918821675E-15, -30.00000000000000000, 26.00000000000000000 ) ) ;
#12460 = CARTESIAN_POINT ( 'NONE',  ( -199.9999999999999716, -40.00000000000003553, 3.000000000000000000 ) ) ;
#12461 = AXIS2_PLACEMENT_3D ( 'NONE', #7016, #9591, #15421 ) ;
#12462 = EDGE_CURVE ( 'NONE', #6128, #13196, #5531, .T. ) ;
#12463 = CARTESIAN_POINT ( 'NONE',  ( 1.846822687350019088, 7.075150813727119292, 10.23524390843941845 ) ) ;
#12464 = FACE_OUTER_BOUND ( 'NONE', #1105, .T. ) ;
#12465 = CARTESIAN_POINT ( 'NONE',  ( 3.950837973638668288, 0.000000000000000000, 0.000000000000000000 ) ) ;
#12466 = CARTESIAN_POINT ( 'NONE',  ( 16.56753206892534891, 0.009369540855502130061, 0.001549402974393180796 ) ) ;
#12467 = CARTESIAN_POINT ( 'NONE',  ( 1.846138399168762101, 6.971848976711011225, 10.30487220521572667 ) ) ;
#12468 = PLANE ( 'NONE',  #6336 ) ;
#12469 = CARTESIAN_POINT ( 'NONE',  ( 1.846138399168762101, -7.646096044339961040, 9.815003036200383946 ) ) ;
#12470 = VERTEX_POINT ( 'NONE', #1363 ) ;
#12471 = EDGE_CURVE ( 'NONE', #18780, #8559, #11597, .T. ) ;
#12472 = ORIENTED_EDGE ( 'NONE', *, *, #10324, .T. ) ;
#12473 = ORIENTED_EDGE ( 'NONE', *, *, #17273, .F. ) ;
#12474 = VERTEX_POINT ( 'NONE', #16379 ) ;
#12475 = CARTESIAN_POINT ( 'NONE',  ( 1.845756295923361323, -9.776763338604659737, 7.694561132136919390 ) ) ;
#12476 =( BOUNDED_SURFACE ( )  B_SPLINE_SURFACE ( 3, 1, ( 
 ( #16495, #9414 ),
 ( #5108, #6167 ),
 ( #16589, #5011 ),
 ( #433, #13618 ) ),
 .UNSPECIFIED., .F., .F., .T. ) 
 B_SPLINE_SURFACE_WITH_KNOTS ( ( 4, 4 ),
 ( 2, 2 ),
 ( 0.000000000000000000, 1.000000000000000000 ),
 ( 0.000000000000000000, 1.000000000000000000 ),
 .UNSPECIFIED. ) 
 GEOMETRIC_REPRESENTATION_ITEM ( )  RATIONAL_B_SPLINE_SURFACE ( (
 ( 1.000000000000000000, 1.000000000000000000),
 ( 0.7792777138730160313, 0.9689936506012927220),
 ( 0.7792777138730160313, 0.9689936506012927220),
 ( 1.000000000000000000, 1.000000000000000000) ) ) 
 REPRESENTATION_ITEM ( '' )  SURFACE ( )  );
#12477 = CARTESIAN_POINT ( 'NONE',  ( 6.236214402462485040, -7.500000000000000000, -16.99999999999999645 ) ) ;
#12478 = CARTESIAN_POINT ( 'NONE',  ( -997.5739745962155212, 0.000000000000000000, 0.000000000000000000 ) ) ;
#12479 = PLANE ( 'NONE',  #7206 ) ;
#12480 = CARTESIAN_POINT ( 'NONE',  ( 0.3132642857406558456, 10.79548167658034608, 8.495623922778108295 ) ) ;
#12481 = CARTESIAN_POINT ( 'NONE',  ( 1.845755665166724846, -11.67596932341231231, -4.296872077620800034 ) ) ;
#12482 = CARTESIAN_POINT ( 'NONE',  ( 1.977436885026782276, -7.806953934146112495, -13.27782258181927233 ) ) ;
#12483 = AXIS2_PLACEMENT_3D ( 'NONE', #18354, #2389, #10821 ) ;
#12484 = DIRECTION ( 'NONE',  ( 1.000000000000000000, -0.000000000000000000, -0.000000000000000000 ) ) ;
#12485 = EDGE_CURVE ( 'NONE', #6301, #14205, #8061, .T. ) ;
#12486 = CARTESIAN_POINT ( 'NONE',  ( 0.4862570985993235340, 7.559321496869426227, 11.67702470553367711 ) ) ;
#12487 = ORIENTED_EDGE ( 'NONE', *, *, #2062, .T. ) ;
#12488 = EDGE_LOOP ( 'NONE', ( #6161, #7409, #5297, #11511, #11192, #9867 ) ) ;
#12489 = VECTOR ( 'NONE', #12868, 1000.000000000000000 ) ;
#12490 = EDGE_CURVE ( 'NONE', #13318, #2558, #11049, .T. ) ;
#12491 = ORIENTED_EDGE ( 'NONE', *, *, #12587, .T. ) ;
#12492 = VERTEX_POINT ( 'NONE', #10933 ) ;
#12493 = CARTESIAN_POINT ( 'NONE',  ( 0.3145734862173242274, -0.3064017202076312341, 13.73540602248381148 ) ) ;
#12494 = CARTESIAN_POINT ( 'NONE',  ( 16.57778382496167424, 0.01018821665058833661, 0.01092721432669112661 ) ) ;
#12495 = CIRCLE ( 'NONE', #4264, 5.000000000000000000 ) ;
#12496 = CARTESIAN_POINT ( 'NONE',  ( 1.846138399168762101, -6.971848976710933954, -10.30487220521577818 ) ) ;
#12497 = CARTESIAN_POINT ( 'NONE',  ( 2.747332970342022840, -14.63517873738952524, 7.289199830147050641 ) ) ;
#12498 = CARTESIAN_POINT ( 'NONE',  ( 16.56753206892534891, 0.001421777558675943985, -0.009389754735542252262 ) ) ;
#12499 = EDGE_LOOP ( 'NONE', ( #5477, #13454, #8113, #13709 ) ) ;
#12500 = CARTESIAN_POINT ( 'NONE',  ( 1.846138399168762989, 10.30487220521570357, 6.971848976711047641 ) ) ;
#12501 = CARTESIAN_POINT ( 'NONE',  ( 1.847380140988742703, -11.86779270755355853, -3.740232970470879881 ) ) ;
#12502 = CARTESIAN_POINT ( 'NONE',  ( -0.7622588538374093226, 7.499999999999999112, -14.39637362139732346 ) ) ;
#12503 = CARTESIAN_POINT ( 'NONE',  ( 3.950837973638675393, 2.591948120961804936, 14.31366178983254578 ) ) ;
#12504 = CARTESIAN_POINT ( 'NONE',  ( 0.3307726912345201886, -8.558645027434195640, -10.76786801061216714 ) ) ;
#12505 = DIRECTION ( 'NONE',  ( -0.000000000000000000, -0.000000000000000000, -1.000000000000000000 ) ) ;
#12506 = CARTESIAN_POINT ( 'NONE',  ( 3.950837973638676281, 10.05648675950141602, -10.51028938476206953 ) ) ;
#12507 = CARTESIAN_POINT ( 'NONE',  ( 0.000000000000000000, 0.000000000000000000, 11.00000000000000000 ) ) ;
#12508 = EDGE_LOOP ( 'NONE', ( #3251, #5481, #16465, #14125 ) ) ;
#12510 = VERTEX_POINT ( 'NONE', #12171 ) ;
#12509 = CARTESIAN_POINT ( 'NONE',  ( -194.9999999999999716, -40.00000000000003553, 3.000000000000000000 ) ) ;
#12511 = CARTESIAN_POINT ( 'NONE',  ( 0.3095370825347233956, 8.444334731364008917, 10.84046130709061373 ) ) ;
#12512 = ADVANCED_FACE ( 'NONE', ( #10735 ), #6433, .T. ) ;
#12513 = EDGE_CURVE ( 'NONE', #12130, #15007, #10832, .T. ) ;
#12514 = ADVANCED_FACE ( 'NONE', ( #514 ), #1893, .T. ) ;
#12515 = ORIENTED_EDGE ( 'NONE', *, *, #7146, .T. ) ;
#12516 = CARTESIAN_POINT ( 'NONE',  ( 3.377929128793386138, 13.92579934231094718, -1.296196549818984911 ) ) ;
#12517 = CARTESIAN_POINT ( 'NONE',  ( 1.847412631396504468, -12.44294644888238821, -0.04315047898448168967 ) ) ;
#12518 = VERTEX_POINT ( 'NONE', #2217 ) ;
#12519 = FACE_OUTER_BOUND ( 'NONE', #10400, .T. ) ;
#12520 = DIRECTION ( 'NONE',  ( 1.224646799147353207E-16, 1.000000000000000000, -0.000000000000000000 ) ) ;
#12521 = CARTESIAN_POINT ( 'NONE',  ( 2.002547531651519996, -10.57595306287296921, 6.845637710436153434 ) ) ;
#12522 = DIRECTION ( 'NONE',  ( -0.000000000000000000, -0.000000000000000000, -1.000000000000000000 ) ) ;
#12523 = ADVANCED_FACE ( 'NONE', ( #1945 ), #8959, .F. ) ;
#12524 = CIRCLE ( 'NONE', #17365, 5.000000000000004441 ) ;
#12525 = DIRECTION ( 'NONE',  ( 0.7635533937278216055, -0.6453904417649387604, -0.02138673900302107828 ) ) ;
#12526 = CARTESIAN_POINT ( 'NONE',  ( 2.320521194583478941, 3.126729093671432480, -15.43440938317170641 ) ) ;
#12527 = DIRECTION ( 'NONE',  ( 0.000000000000000000, 0.000000000000000000, -1.000000000000000000 ) ) ;
#12529 = VERTEX_POINT ( 'NONE', #16655 ) ;
#12528 = CARTESIAN_POINT ( 'NONE',  ( 3.950837973638668288, 0.000000000000000000, 0.000000000000000000 ) ) ;
#12530 = DIRECTION ( 'NONE',  ( -0.000000000000000000, -1.000000000000000000, -0.000000000000000000 ) ) ;
#12531 = CARTESIAN_POINT ( 'NONE',  ( 0.3720661004400037664, 3.575426119359183197, 13.34435358167253938 ) ) ;
#12532 = CARTESIAN_POINT ( 'NONE',  ( 2.636624412714236865, 0.000000000000000000, -16.06066017081991149 ) ) ;
#12533 = CARTESIAN_POINT ( 'NONE',  ( 2.636624412714292376, 11.60464335004048309, 11.10302021257707850 ) ) ;
#12534 = ORIENTED_EDGE ( 'NONE', *, *, #6952, .T. ) ;
#12535 = EDGE_LOOP ( 'NONE', ( #18662, #7627, #13029, #13121 ) ) ;
#12536 = EDGE_CURVE ( 'NONE', #2858, #18187, #16221, .T. ) ;
#12537 = DIRECTION ( 'NONE',  ( 0.7561779333270775005, 0.6322161072786955938, -0.1688126975276531827 ) ) ;
#12538 = EDGE_CURVE ( 'NONE', #18705, #5896, #15128, .T. ) ;
#12539 = APPLICATION_CONTEXT ( 'automotive_design' ) ;
#12540 = CARTESIAN_POINT ( 'NONE',  ( 16.56753206892534891, -0.004253784598196824578, -0.008490833999797990639 ) ) ;
#12541 = ORIENTED_EDGE ( 'NONE', *, *, #2600, .T. ) ;
#12542 = CARTESIAN_POINT ( 'NONE',  ( 1.918918678667071775, -0.6348738215464356793, -12.49849921341423986 ) ) ;
#12543 = CARTESIAN_POINT ( 'NONE',  ( 2.002547531651519996, 6.845637710436341727, -10.57595306287284842 ) ) ;
#12544 = VECTOR ( 'NONE', #16699, 1000.000000000000114 ) ;
#12545 = CARTESIAN_POINT ( 'NONE',  ( 1.847412631396500249, -10.04119192206681177, -7.348689888531952263 ) ) ;
#12546 = CARTESIAN_POINT ( 'NONE',  ( -112.9592833967653149, -82.42962774651277869, -85.91158569379400944 ) ) ;
#12547 = LINE ( 'NONE', #12366, #2342 ) ;
#12548 = EDGE_CURVE ( 'NONE', #13259, #5916, #2771, .T. ) ;
#12549 = B_SPLINE_CURVE_WITH_KNOTS ( 'NONE', 3,
 ( #10667, #16498, #5014, #3286, #3485, #14955 ),
 .UNSPECIFIED., .F., .F.,
 ( 4, 2, 4 ),
 ( 0.000000000000000000, 0.001500839035891548753, 0.003001678071783097507 ),
 .UNSPECIFIED. ) ;
#12550 = DIRECTION ( 'NONE',  ( -1.000000000000000000, -1.298018465182616140E-16, -0.000000000000000000 ) ) ;
#12551 = SHAPE_DEFINITION_REPRESENTATION ( #7225, #18049 ) ;
#12552 = CARTESIAN_POINT ( 'NONE',  ( 1.861628059977341154, 7.751680370225533245, -9.751736252960284901 ) ) ;
#12553 = CARTESIAN_POINT ( 'NONE',  ( 0.3142011359265348691, -12.94258167753015520, 4.608101617236726177 ) ) ;
#12554 = LINE ( 'NONE', #5293, #9276 ) ;
#12555 = CARTESIAN_POINT ( 'NONE',  ( 20.00000000000000711, -40.00000000000000000, 3.000000000000000000 ) ) ;
#12556 = VECTOR ( 'NONE', #12527, 1000.000000000000000 ) ;
#12557 = CARTESIAN_POINT ( 'NONE',  ( 2.320521194583335500, -13.71278319228129483, -7.743190876766059105 ) ) ;
#12558 = CARTESIAN_POINT ( 'NONE',  ( 0.3137051932979757485, -7.698472063774552510, 11.37800749014128421 ) ) ;
#12559 = ORIENTED_EDGE ( 'NONE', *, *, #1919, .F. ) ;
#12560 = VERTEX_POINT ( 'NONE', #7885 ) ;
#12561 = ADVANCED_FACE ( 'NONE', ( #7972 ), #13696, .T. ) ;
#12562 = EDGE_LOOP ( 'NONE', ( #11144, #8041, #7304, #11289 ) ) ;
#12563 = ORIENTED_EDGE ( 'NONE', *, *, #10629, .F. ) ;
#12564 = CARTESIAN_POINT ( 'NONE',  ( 1.846138399168762101, -9.815003036200465658, 7.646096044339859787 ) ) ;
#12565 = EDGE_CURVE ( 'NONE', #4649, #8892, #13475, .T. ) ;
#12566 = CARTESIAN_POINT ( 'NONE',  ( -0.6933513387705726450, -7.500000000000003553, -14.36029122898769117 ) ) ;
#12567 = CARTESIAN_POINT ( 'NONE',  ( 25.00000000000000000, 7.499999999999999112, -22.00000000000000000 ) ) ;
#12568 = CARTESIAN_POINT ( 'NONE',  ( 1.977228804422057840, -7.806978995470733373, 13.27756617201263545 ) ) ;
#12569 = EDGE_CURVE ( 'NONE', #3637, #11886, #9393, .T. ) ;
#12570 = DIRECTION ( 'NONE',  ( 0.000000000000000000, 0.000000000000000000, 1.000000000000000000 ) ) ;
#12571 = CARTESIAN_POINT ( 'NONE',  ( 1.342453679581834924, -5.476372339890114738, 13.74702459364882401 ) ) ;
#12572 = AXIS2_PLACEMENT_3D ( 'NONE', #17772, #16617, #4676 ) ;
#12573 = CARTESIAN_POINT ( 'NONE',  ( 0.3148208552358916501, -12.99355031785208681, 4.463611911212169936 ) ) ;
#12574 = LINE ( 'NONE', #12947, #13028 ) ;
#12575 = ORIENTED_EDGE ( 'NONE', *, *, #15429, .T. ) ;
#12576 = ORIENTED_EDGE ( 'NONE', *, *, #6371, .F. ) ;
#12577 = ORIENTED_EDGE ( 'NONE', *, *, #12548, .T. ) ;
#12578 = ORIENTED_EDGE ( 'NONE', *, *, #12286, .F. ) ;
#12579 =( BOUNDED_SURFACE ( )  B_SPLINE_SURFACE ( 3, 1, ( 
 ( #14719, #10332 ),
 ( #11863, #16161 ),
 ( #1731, #12157 ),
 ( #15110, #10720 ) ),
 .UNSPECIFIED., .F., .F., .T. ) 
 B_SPLINE_SURFACE_WITH_KNOTS ( ( 4, 4 ),
 ( 2, 2 ),
 ( 0.000000000000000000, 1.000000000000000000 ),
 ( 0.000000000000000000, 1.000000000000000000 ),
 .UNSPECIFIED. ) 
 GEOMETRIC_REPRESENTATION_ITEM ( )  RATIONAL_B_SPLINE_SURFACE ( (
 ( 1.000000000000000000, 1.000000000000000000),
 ( 0.9933953342250436691, 0.8357391271907733676),
 ( 0.9933953342250436691, 0.8357391271907733676),
 ( 1.000000000000000000, 1.000000000000000000) ) ) 
 REPRESENTATION_ITEM ( '' )  SURFACE ( )  );
#12580 = CARTESIAN_POINT ( 'NONE',  ( 2.747332970342022840, 11.45495994260717865, 11.66639548242811486 ) ) ;
#12581 = FACE_OUTER_BOUND ( 'NONE', #18320, .T. ) ;
#12582 = CARTESIAN_POINT ( 'NONE',  ( 0.4754618798421171855, -12.98792082933648118, 5.007009103465197342 ) ) ;
#12583 = FACE_BOUND ( 'NONE', #9869, .T. ) ;
#12584 = FILL_AREA_STYLE_COLOUR ( '', #11225 ) ;
#12585 = VERTEX_POINT ( 'NONE', #413 ) ;
#12586 = CARTESIAN_POINT ( 'NONE',  ( 5.923783695726432263, 7.500000000000000000, -16.97504159551249359 ) ) ;
#12587 = EDGE_CURVE ( 'NONE', #9233, #15002, #12075, .T. ) ;
#12588 = CARTESIAN_POINT ( 'NONE',  ( 0.8740764193766107359, 7.708542792189345683, 12.04241474977975557 ) ) ;
#12589 = CARTESIAN_POINT ( 'NONE',  ( 6.437519407326084853, 7.499999999999865885, -12.20843479742065441 ) ) ;
#12590 = CARTESIAN_POINT ( 'NONE',  ( 6.000000000000000000, 20.00000000000000000, 4.000000000000000000 ) ) ;
#12591 = CIRCLE ( 'NONE', #4357, 14.54644660717763927 ) ;
#12592 = DIRECTION ( 'NONE',  ( 0.000000000000000000, 0.000000000000000000, -1.000000000000000000 ) ) ;
#12593 = ADVANCED_FACE ( 'NONE', ( #9199 ), #1249, .F. ) ;
#12594 = CARTESIAN_POINT ( 'NONE',  ( 22.75000000000000000, 0.000000000000000000, 0.000000000000000000 ) ) ;
#12595 = CARTESIAN_POINT ( 'NONE',  ( 16.56753206892534891, 0.004253784598196760393, 0.008490833999798020129 ) ) ;
#12596 = CARTESIAN_POINT ( 'NONE',  ( 0.3150692679895995552, 11.02465386701228844, 8.199139630396045320 ) ) ;
#12597 = ORIENTED_EDGE ( 'NONE', *, *, #3757, .F. ) ;
#12599 = VERTEX_POINT ( 'NONE', #18449 ) ;
#12598 = CARTESIAN_POINT ( 'NONE',  ( 16.56782317627811096, 0.005492611183757310257, -0.008141063682853423578 ) ) ;
#12600 = DIRECTION ( 'NONE',  ( -1.000000000000000000, -0.000000000000000000, -0.000000000000000000 ) ) ;
#12601 = FACE_OUTER_BOUND ( 'NONE', #12225, .T. ) ;
#12602 = AXIS2_PLACEMENT_3D ( 'NONE', #12170, #17999, #316 ) ;
#12603 = VERTEX_POINT ( 'NONE', #5535 ) ;
#12604 = LINE ( 'NONE', #11099, #905 ) ;
#12605 = CARTESIAN_POINT ( 'NONE',  ( 2.636624412717140764, -2.862162146982851763, -15.80357026013259514 ) ) ;
#12606 =( NAMED_UNIT ( * ) PLANE_ANGLE_UNIT ( ) SI_UNIT ( $, .RADIAN. ) );
#12607 = VERTEX_POINT ( 'NONE', #6995 ) ;
#12608 = CARTESIAN_POINT ( 'NONE',  ( 1.977436885027552549, 15.04044112860454518, -3.321781585407754811 ) ) ;
#12609 = CARTESIAN_POINT ( 'NONE',  ( 0.3137051932979809665, -13.20008686438108647, 3.805684345189735307 ) ) ;
#12610 = CARTESIAN_POINT ( 'NONE',  ( -194.9999999999999716, -5.000000000000024869, -153.7432847437423789 ) ) ;
#12611 = DIRECTION ( 'NONE',  ( 1.000000000000000000, 0.000000000000000000, 0.000000000000000000 ) ) ;
#12612 = ADVANCED_FACE ( 'NONE', ( #17030, #9569, #18362 ), #17205, .T. ) ;
#12613 = ADVANCED_FACE ( 'NONE', ( #3739 ), #11042, .F. ) ;
#12614 = CARTESIAN_POINT ( 'NONE',  ( -30.00000000000000711, 20.00000000000000000, 3.000000000000000000 ) ) ;
#12615 = EDGE_CURVE ( 'NONE', #16044, #2096, #18358, .T. ) ;
#12616 = CIRCLE ( 'NONE', #14142, 14.54644660717763927 ) ;
#12617 = CARTESIAN_POINT ( 'NONE',  ( 16.57210152137263393, -0.0006600038696347039187, 0.01453130299868522074 ) ) ;
#12618 = CIRCLE ( 'NONE', #2845, 16.06066017081991149 ) ;
#12620 = VERTEX_POINT ( 'NONE', #5362 ) ;
#12619 = FACE_OUTER_BOUND ( 'NONE', #17651, .T. ) ;
#12621 = CARTESIAN_POINT ( 'NONE',  ( 16.58200780006414732, -0.01080144354108868512, -0.002844973367391535370 ) ) ;
#12622 = CARTESIAN_POINT ( 'NONE',  ( 1.977436885026099711, -15.33079650480437550, -1.488549889122204650 ) ) ;
#12623 = CARTESIAN_POINT ( 'NONE',  ( 0.3148213771069355293, -4.026433757158891957, -13.13560149728604998 ) ) ;
#12624 = EDGE_LOOP ( 'NONE', ( #3826, #1835, #7404, #11052 ) ) ;
#12625 = CARTESIAN_POINT ( 'NONE',  ( 8.438534575730034959, 6.454982381540289360, 2.341351102130301065 ) ) ;
#12626 = CARTESIAN_POINT ( 'NONE',  ( 0.3150690434770175852, 0.1531837610935626592, -13.73846430619029313 ) ) ;
#12627 = ORIENTED_EDGE ( 'NONE', *, *, #15837, .F. ) ;
#12628 = CARTESIAN_POINT ( 'NONE',  ( 3.950837973638677170, 13.10350451991849141, -6.316429227969337923 ) ) ;
#12629 = CARTESIAN_POINT ( 'NONE',  ( 0.3720661004400040439, -13.79610186261030513, 0.7231997263364323691 ) ) ;
#12630 = CIRCLE ( 'NONE', #14161, 3.999999999999993339 ) ;
#12631 = SURFACE_STYLE_USAGE ( .BOTH. , #9410 ) ;
#12632 = PRODUCT_DEFINITION_FORMATION_WITH_SPECIFIED_SOURCE ( 'ANY', '', #11962, .NOT_KNOWN. ) ;
#12633 = DIRECTION ( 'NONE',  ( 0.000000000000000000, 0.000000000000000000, 1.000000000000000000 ) ) ;
#12634 = FACE_OUTER_BOUND ( 'NONE', #8636, .T. ) ;
#12635 = UNCERTAINTY_MEASURE_WITH_UNIT (LENGTH_MEASURE( 1.000000000000000082E-05 ), #8265, 'distance_accuracy_value', 'NONE');
#12636 = ADVANCED_FACE ( 'NONE', ( #18274 ), #10114, .T. ) ;
#12637 = EDGE_CURVE ( 'NONE', #17016, #5495, #17113, .T. ) ;
#12638 = EDGE_CURVE ( 'NONE', #13171, #13464, #15399, .T. ) ;
#12639 = DIRECTION ( 'NONE',  ( 0.000000000000000000, 0.000000000000000000, 1.000000000000000000 ) ) ;
#12640 = APPLICATION_PROTOCOL_DEFINITION ( 'draft international standard', 'automotive_design', 1998, #7680 ) ;
#12641 = ADVANCED_FACE ( 'NONE', ( #2307 ), #8459, .F. ) ;
#12642 = FILL_AREA_STYLE ('',( #5470 ) ) ;
#12643 = FACE_OUTER_BOUND ( 'NONE', #7818, .T. ) ;
#12644 = CARTESIAN_POINT ( 'NONE',  ( 16.56782317627811096, 0.009439921864426886397, -0.002708056627498675335 ) ) ;
#12645 = CARTESIAN_POINT ( 'NONE',  ( 3.950837973638677170, -1.958075594453692503, -14.41405733518062959 ) ) ;
#12646 = CARTESIAN_POINT ( 'NONE',  ( 1.847380140988742925, 3.949801494731767892, 11.79969976631073081 ) ) ;
#12647 = DIRECTION ( 'NONE',  ( -1.601283208593975514E-16, 1.000000000000000000, -0.000000000000000000 ) ) ;
#12648 = VECTOR ( 'NONE', #14611, 1000.000000000000000 ) ;
#12649 = DIRECTION ( 'NONE',  ( 0.000000000000000000, 0.000000000000000000, -1.000000000000000000 ) ) ;
#12650 = DIRECTION ( 'NONE',  ( -0.000000000000000000, 1.000000000000000000, -0.000000000000000000 ) ) ;
#12651 = B_SPLINE_CURVE_WITH_KNOTS ( 'NONE', 3,
 ( #734, #15260, #561, #6566, #16790, #4854 ),
 .UNSPECIFIED., .F., .F.,
 ( 4, 2, 4 ),
 ( 0.000000000000000000, 0.001656992708823243950, 0.003313985417646487033 ),
 .UNSPECIFIED. ) ;
#12652 = ORIENTED_EDGE ( 'NONE', *, *, #13309, .F. ) ;
#12653 = CONICAL_SURFACE ( 'NONE', #13573, 8.767949192431130356, 1.308996938995746318 ) ;
#12654 = ORIENTED_EDGE ( 'NONE', *, *, #9025, .F. ) ;
#12655 = AXIS2_PLACEMENT_3D ( 'NONE', #1299, #18596, #9995 ) ;
#12656 = ORIENTED_EDGE ( 'NONE', *, *, #5609, .F. ) ;
#12657 = ORIENTED_EDGE ( 'NONE', *, *, #14548, .T. ) ;
#12658 = FACE_OUTER_BOUND ( 'NONE', #11563, .T. ) ;
#12659 = CARTESIAN_POINT ( 'NONE',  ( 0.3148213771069354738, 13.13560149728606419, -4.026433757158845772 ) ) ;
#12660 = AXIS2_PLACEMENT_3D ( 'NONE', #11970, #1639, #17507 ) ;
#12661 = LINE ( 'NONE', #11522, #15411 ) ;
#12662 = CARTESIAN_POINT ( 'NONE',  ( 3.074695600507753479, -6.754521329825609932, -14.01296402267891317 ) ) ;
#12663 = CIRCLE ( 'NONE', #474, 5.000000000000000000 ) ;
#12664 = VECTOR ( 'NONE', #931, 1000.000000000000000 ) ;
#12665 =( NAMED_UNIT ( * ) PLANE_ANGLE_UNIT ( ) SI_UNIT ( $, .RADIAN. ) );
#12666 = CARTESIAN_POINT ( 'NONE',  ( 0.3132635586635982849, 7.641727604904055227, -11.41586812343481583 ) ) ;
#12667 = B_SPLINE_CURVE_WITH_KNOTS ( 'NONE', 3,
 ( #14067, #16660, #10837, #16843, #9489, #10939 ),
 .UNSPECIFIED., .F., .F.,
 ( 4, 2, 4 ),
 ( 8.673617379884035472E-19, 0.0001828790815886931534, 0.0003657581631773854395 ),
 .UNSPECIFIED. ) ;
#12668 = EDGE_CURVE ( 'NONE', #12087, #11329, #15303, .T. ) ;
#12669 = DIRECTION ( 'NONE',  ( -0.7561779333270775005, 0.6534392409364818688, -0.03481510524965020920 ) ) ;
#12670 = CARTESIAN_POINT ( 'NONE',  ( -33.49999999999999289, -12.50000000000000178, 6.000000000000000000 ) ) ;
#12671 = ORIENTED_EDGE ( 'NONE', *, *, #773, .F. ) ;
#12672 = ORIENTED_EDGE ( 'NONE', *, *, #6224, .F. ) ;
#12673 = VERTEX_POINT ( 'NONE', #8334 ) ;
#12674 = AXIS2_PLACEMENT_3D ( 'NONE', #2988, #15908, #8553 ) ;
#12675 = ORIENTED_EDGE ( 'NONE', *, *, #129, .F. ) ;
#12676 = AXIS2_PLACEMENT_3D ( 'NONE', #6947, #4260, #5575 ) ;
#12677 = DIRECTION ( 'NONE',  ( 0.000000000000000000, 0.000000000000000000, 1.000000000000000000 ) ) ;
#12678 = EDGE_CURVE ( 'NONE', #3393, #5038, #6928, .T. ) ;
#12679 = FACE_OUTER_BOUND ( 'NONE', #6883, .T. ) ;
#12680 = FACE_OUTER_BOUND ( 'NONE', #13693, .T. ) ;
#12681 = DIRECTION ( 'NONE',  ( -0.000000000000000000, -0.000000000000000000, -1.000000000000000000 ) ) ;
#12682 =( NAMED_UNIT ( * ) PLANE_ANGLE_UNIT ( ) SI_UNIT ( $, .RADIAN. ) );
#12683 = ORIENTED_EDGE ( 'NONE', *, *, #14449, .T. ) ;
#12684 = CARTESIAN_POINT ( 'NONE',  ( 1.847461586945732037, 10.08650590720936258, 7.286856109515091440 ) ) ;
#12685 = CARTESIAN_POINT ( 'NONE',  ( 16.56872352241294521, 0.004564908236399969378, -0.009382111268607383134 ) ) ;
#12686 = CARTESIAN_POINT ( 'NONE',  ( 5.763005853485449137, 3.979914285031491694, -11.99999999870348688 ) ) ;
#12687 = PRODUCT_DEFINITION ( 'UNKNOWN', '', #10508, #15169 ) ;
#12688 = EDGE_CURVE ( 'NONE', #4997, #18304, #14149, .T. ) ;
#12689 = FACE_OUTER_BOUND ( 'NONE', #7244, .T. ) ;
#12690 = FACE_BOUND ( 'NONE', #8253, .T. ) ;
#12691 = CARTESIAN_POINT ( 'NONE',  ( 1.560000000000000053, 0.000000000000000000, 2.999999999999998668 ) ) ;
#12692 = CIRCLE ( 'NONE', #7222, 1.000000000000000000 ) ;
#12693 = CARTESIAN_POINT ( 'NONE',  ( 8.522092701127531811, -6.946128462138598358, 0.3779863304870977325 ) ) ;
#12694 = CIRCLE ( 'NONE', #4458, 5.000000000000004441 ) ;
#12695 = VERTEX_POINT ( 'NONE', #18547 ) ;
#12697 = ORIENTED_EDGE ( 'NONE', *, *, #5855, .T. ) ;
#12696 = DIRECTION ( 'NONE',  ( 0.000000000000000000, 0.000000000000000000, 1.000000000000000000 ) ) ;
#12698 = CARTESIAN_POINT ( 'NONE',  ( 0.3132635586635980629, 4.743936529203241825, 12.89236642382223508 ) ) ;
#12699 = CARTESIAN_POINT ( 'NONE',  ( 16.56782317627811096, 0.006045301465876630996, 0.007739510688078455984 ) ) ;
#12700 = ADVANCED_FACE ( 'NONE', ( #9837, #15671 ), #2572, .F. ) ;
#12701 = EDGE_LOOP ( 'NONE', ( #16887, #4249, #11602, #13509 ) ) ;
#12702 = DIRECTION ( 'NONE',  ( -1.000000000000000000, 0.000000000000000000, 0.000000000000000000 ) ) ;
#12703 = CARTESIAN_POINT ( 'NONE',  ( -6.437519407326167453, -7.499999999999735323, -12.20843479742017657 ) ) ;
#12704 = COLOUR_RGB ( '', 0.72549020, 0.75294118, 0.79215686) ;
#12705 = FACE_OUTER_BOUND ( 'NONE', #9230, .T. ) ;
#12706 = ORIENTED_EDGE ( 'NONE', *, *, #5134, .F. ) ;
#12707 = CARTESIAN_POINT ( 'NONE',  ( 1.847247051441596621, -7.448813758297236909, 9.967131402978164800 ) ) ;
#12708 = EDGE_CURVE ( 'NONE', #14346, #12958, #10135, .T. ) ;
#12709 = DIRECTION ( 'NONE',  ( -2.891205793294679312E-16, -1.000000000000000000, 0.000000000000000000 ) ) ;
#12710 = CARTESIAN_POINT ( 'NONE',  ( 1.846822687350018866, 12.43915556955403900, 0.2922081769260583273 ) ) ;
#12711 = DIRECTION ( 'NONE',  ( -1.000000000000000000, 1.387778780781445478E-15, 0.000000000000000000 ) ) ;
#12712 = CARTESIAN_POINT ( 'NONE',  ( 1.560000000000000053, -1.299038105676658450, -0.7500000000000007772 ) ) ;
#12713 = AXIS2_PLACEMENT_3D ( 'NONE', #11187, #13143, #7331 ) ;
#12714 = CIRCLE ( 'NONE', #17610, 5.000000000000000888 ) ;
#12715 = PRESENTATION_LAYER_ASSIGNMENT (  '', '', ( #9957 ) ) ;
#12716 = CARTESIAN_POINT ( 'NONE',  ( 16.56872352241294521, 0.009207754980063749192, 0.004907101719994666836 ) ) ;
#12717 = AXIS2_PLACEMENT_3D ( 'NONE', #14887, #10032, #3314 ) ;
#12718 = CARTESIAN_POINT ( 'NONE',  ( 0.3095370825347224519, 8.444334731364161684, -10.84046130709049471 ) ) ;
#12720 = ORIENTED_EDGE ( 'NONE', *, *, #2804, .T. ) ;
#12719 = DIRECTION ( 'NONE',  ( -0.7561779333270775005, -0.6322161072786931513, -0.1688126975276622865 ) ) ;
#12721 = CARTESIAN_POINT ( 'NONE',  ( 0.4862570985993235340, 0.7479633556564388996, -13.89016912371016765 ) ) ;
#12722 = B_SPLINE_CURVE_WITH_KNOTS ( 'NONE', 3,
 ( #9561, #6795, #16921, #6886, #15571, #3734 ),
 .UNSPECIFIED., .F., .F.,
 ( 4, 2, 4 ),
 ( 0.000000000000000000, 0.001656992708822367915, 0.003313985417644735830 ),
 .UNSPECIFIED. ) ;
#12723 = VECTOR ( 'NONE', #13937, 1000.000000000000000 ) ;
#12724 = AXIS2_PLACEMENT_3D ( 'NONE', #1350, #7195, #11587 ) ;
#12725 = CARTESIAN_POINT ( 'NONE',  ( 0.3150692679895995552, -13.01874238516607285, -4.391039771493804089 ) ) ;
#12726 = EDGE_CURVE ( 'NONE', #10356, #14041, #6007, .T. ) ;
#12727 = ORIENTED_EDGE ( 'NONE', *, *, #18129, .F. ) ;
#12728 = CARTESIAN_POINT ( 'NONE',  ( -194.9999999999999716, -5.000000000000024869, 6.000000000000000000 ) ) ;
#12729 = TOROIDAL_SURFACE ( 'NONE', #4500, 3.499999999999992450, 0.5000000000000000000 ) ;
#12730 = ORIENTED_EDGE ( 'NONE', *, *, #4932, .F. ) ;
#12731 = CIRCLE ( 'NONE', #6946, 5.000000000000000000 ) ;
#12732 = CARTESIAN_POINT ( 'NONE',  ( 1.560000000000000053, 1.299038105676658228, 0.7500000000000009992 ) ) ;
#12733 = CARTESIAN_POINT ( 'NONE',  ( 2.320521194583478941, 3.126729093671432480, -15.43440938317170641 ) ) ;
#12734 = CARTESIAN_POINT ( 'NONE',  ( 0.3151930723728453843, -4.318364831037682094, 13.04315954105013198 ) ) ;
#12735 = CARTESIAN_POINT ( 'NONE',  ( 0.4862570985993235340, -10.79774104611379215, 8.769551628660700260 ) ) ;
#12736 = CARTESIAN_POINT ( 'NONE',  ( 8.438534575730034959, -1.899950616255142277, -6.598402093327899287 ) ) ;
#12737 = ORIENTED_EDGE ( 'NONE', *, *, #8215, .T. ) ;
#12738 = CONTEXT_DEPENDENT_SHAPE_REPRESENTATION ( #7936, #4318 ) ;
#12739 = CARTESIAN_POINT ( 'NONE',  ( 0.3939875929385656117, -13.34133634968952720, -3.598491969338368346 ) ) ;
#12740 = CARTESIAN_POINT ( 'NONE',  ( 0.3142014840576517476, -13.17932813834297434, 3.879477880151391833 ) ) ;
#12741 = CARTESIAN_POINT ( 'NONE',  ( 0.4384471787762845851, -4.978024343488958614, -12.93784327393178302 ) ) ;
#12742 = CARTESIAN_POINT ( 'NONE',  ( 2.636624412715137922, -14.46769361191291559, 6.973567714907789927 ) ) ;
#12743 = FACE_OUTER_BOUND ( 'NONE', #17770, .T. ) ;
#12744 = ORIENTED_EDGE ( 'NONE', *, *, #5440, .T. ) ;
#12745 = CARTESIAN_POINT ( 'NONE',  ( 0.4754618798421162973, -3.583352865732763792, 13.45049478164058776 ) ) ;
#12746 = CARTESIAN_POINT ( 'NONE',  ( 2.636624412717140764, -2.862162146982851763, -15.80357026013259514 ) ) ;
#12747 = EDGE_LOOP ( 'NONE', ( #10185, #11444, #1558, #11453 ) ) ;
#12748 = ADVANCED_FACE ( 'NONE', ( #5821 ), #15868, .T. ) ;
#12749 = EDGE_CURVE ( 'NONE', #6964, #16555, #198, .T. ) ;
#12750 = EDGE_CURVE ( 'NONE', #11838, #1858, #1926, .T. ) ;
#12751 = ORIENTED_EDGE ( 'NONE', *, *, #10512, .F. ) ;
#12752 = EDGE_LOOP ( 'NONE', ( #4554, #6308, #14344, #15848, #14304, #2019, #17942, #8199, #4596, #4403, #3453, #14409, #10184, #14580, #14442, #7329, #9759, #15537, #16783, #12204, #6538, #4874, #12292, #518, #12952, #10772, #13427, #6697, #7959, #4401, #16210, #2739, #9631, #17183, #4975, #2428, #1680, #17256, #861, #17604, #7575, #17190, #13301, #3037, #4744, #10945, #16941, #2167, #11713, #5371, #7554, #9293, #7043, #16939, #11081, #4973, #4938, #9572, #10281, #10799, #17122, #4936, #11586, #12214 ) ) ;
#12753 = ORIENTED_EDGE ( 'NONE', *, *, #9404, .F. ) ;
#12754 = LINE ( 'NONE', #11424, #7526 ) ;
#12755 = CARTESIAN_POINT ( 'NONE',  ( 1.847034903785818694, -9.929438108952092890, -7.498375632854726192 ) ) ;
#12756 = PLANE ( 'NONE',  #5949 ) ;
#12757 = CARTESIAN_POINT ( 'NONE',  ( 1.861628059977344263, 6.879051339207292948, 10.38573835516714716 ) ) ;
#12758 = VECTOR ( 'NONE', #3274, 1000.000000000000227 ) ;
#12759 =( LENGTH_UNIT ( ) NAMED_UNIT ( * ) SI_UNIT ( .MILLI., .METRE. ) );
#12760 = CARTESIAN_POINT ( 'NONE',  ( 8.522092701127531811, -1.786985377232080285, 6.722964936702092054 ) ) ;
#12761 = CARTESIAN_POINT ( 'NONE',  ( 2.747332970342022840, 2.705255688518072965, -16.12459247543623064 ) ) ;
#12762 = B_SPLINE_CURVE_WITH_KNOTS ( 'NONE', 3,
 ( #13348, #1887, #9236, #260, #4655, #17847 ),
 .UNSPECIFIED., .F., .F.,
 ( 4, 2, 4 ),
 ( 8.673617379884035472E-19, 0.001500839035891551572, 0.003001678071783102277 ),
 .UNSPECIFIED. ) ;
#12763 = CARTESIAN_POINT ( 'NONE',  ( 16.57210152137263393, -0.009075239946108286035, 0.01136813053532071717 ) ) ;
#12764 = CARTESIAN_POINT ( 'NONE',  ( 1.959283090834855745, -12.53713130127478337, 0.6676170829051779609 ) ) ;
#12765 = VERTEX_POINT ( 'NONE', #10035 ) ;
#12766 = VERTEX_POINT ( 'NONE', #2760 ) ;
#12767 = VERTEX_POINT ( 'NONE', #17698 ) ;
#12768 = ORIENTED_EDGE ( 'NONE', *, *, #8846, .T. ) ;
#12769 = EDGE_CURVE ( 'NONE', #13818, #18306, #1672, .T. ) ;
#12770 = CARTESIAN_POINT ( 'NONE',  ( 16.56822296793089322, -0.009847136207496290372, -0.002414375228568220195 ) ) ;
#12771 = CARTESIAN_POINT ( 'NONE',  ( 1.847412631396500249, 10.09191835241973934, -7.278870946904142158 ) ) ;
#12772 = DIRECTION ( 'NONE',  ( 0.000000000000000000, 0.000000000000000000, 1.000000000000000000 ) ) ;
#12773 = SURFACE_SIDE_STYLE ('',( #8384 ) ) ;
#12774 = EDGE_CURVE ( 'NONE', #6674, #12889, #11954, .T. ) ;
#12775 = VERTEX_POINT ( 'NONE', #8985 ) ;
#12776 = CARTESIAN_POINT ( 'NONE',  ( 0.4754618798421162973, 8.775436892861270266, -10.80499583390503382 ) ) ;
#12777 = CARTESIAN_POINT ( 'NONE',  ( 2.636624412714756005, -2.161493821597335607, 15.91454522070219113 ) ) ;
#12778 = CARTESIAN_POINT ( 'NONE',  ( 3.324307330593150756, 6.179741886604479539, -11.99999999169344633 ) ) ;
#12779 = CARTESIAN_POINT ( 'NONE',  ( 1.254009781011695468, -14.24044713813331597, -3.563484327698402510 ) ) ;
#12780 = EDGE_CURVE ( 'NONE', #9066, #8143, #12835, .T. ) ;
#12781 = CARTESIAN_POINT ( 'NONE',  ( 2.426025403784448642, 2.168404344971008868E-16, 0.000000000000000000 ) ) ;
#12782 = CARTESIAN_POINT ( 'NONE',  ( 1.846138399168762101, -3.446241763652916124, -11.95493567637853971 ) ) ;
#12783 = FACE_OUTER_BOUND ( 'NONE', #4054, .T. ) ;
#12784 = CARTESIAN_POINT ( 'NONE',  ( 8.522092701127531811, 1.786985377232031436, 6.722964936702105376 ) ) ;
#12785 = ORIENTED_EDGE ( 'NONE', *, *, #926, .T. ) ;
#12787 = ORIENTED_EDGE ( 'NONE', *, *, #13966, .F. ) ;
#12786 = CARTESIAN_POINT ( 'NONE',  ( -194.9999999999999716, -40.00000000000003553, 3.000000000000000000 ) ) ;
#12788 = CARTESIAN_POINT ( 'NONE',  ( 2.747332970342022840, -14.63517873738941866, -7.289199830147261139 ) ) ;
#12789 = CONICAL_SURFACE ( 'NONE', #7942, 2.055000000000000160, 0.7853981633974468357 ) ;
#12790 = EDGE_CURVE ( 'NONE', #18142, #5568, #5096, .T. ) ;
#12791 = CARTESIAN_POINT ( 'NONE',  ( 3.950837973638668288, 0.000000000000000000, 0.000000000000000000 ) ) ;
#12792 = VERTEX_POINT ( 'NONE', #11859 ) ;
#12793 = CARTESIAN_POINT ( 'NONE',  ( 1.321128355694181398E-14, -9.013167318348349610, 25.01316734529530095 ) ) ;
#12794 = EDGE_CURVE ( 'NONE', #10403, #14985, #993, .T. ) ;
#12795 = EDGE_CURVE ( 'NONE', #8319, #5753, #8700, .T. ) ;
#12796 = CARTESIAN_POINT ( 'NONE',  ( 1.846138399168762101, -12.43476674860266229, -0.4167076046096845898 ) ) ;
#12797 = CARTESIAN_POINT ( 'NONE',  ( 2.747332970342022840, 16.12459247543629814, -2.705255688517677282 ) ) ;
#12798 = B_SPLINE_CURVE_WITH_KNOTS ( 'NONE', 3,
 ( #16822, #3914, #3724, #8227 ),
 .UNSPECIFIED., .F., .F.,
 ( 4, 4 ),
 ( 5.210130127421859526E-17, 0.002004993803842660023 ),
 .UNSPECIFIED. ) ;
#12799 = SURFACE_STYLE_USAGE ( .BOTH. , #6986 ) ;
#12800 = ORIENTED_EDGE ( 'NONE', *, *, #10426, .T. ) ;
#12801 = CARTESIAN_POINT ( 'NONE',  ( -199.9999999999999716, 9.999999999999973355, 3.000000000000000000 ) ) ;
#12802 = VECTOR ( 'NONE', #9360, 1000.000000000000000 ) ;
#12803 = CARTESIAN_POINT ( 'NONE',  ( 0.000000000000000000, 0.000000000000000000, 0.000000000000000000 ) ) ;
#12804 = CARTESIAN_POINT ( 'NONE',  ( 0.3132642857406529591, -13.72733058964894681, -0.5276792104583708509 ) ) ;
#12805 = DIRECTION ( 'NONE',  ( 0.000000000000000000, 0.000000000000000000, 1.000000000000000000 ) ) ;
#12806 = LINE ( 'NONE', #11476, #768 ) ;
#12807 = EDGE_CURVE ( 'NONE', #1302, #10558, #13763, .T. ) ;
#12808 = CARTESIAN_POINT ( 'NONE',  ( 0.4754618798421171855, -12.98792082933648118, 5.007009103465197342 ) ) ;
#12809 = CARTESIAN_POINT ( 'NONE',  ( 16.56782317627811096, 0.009814734722106368062, -0.0003415813796015080314 ) ) ;
#12811 = ORIENTED_EDGE ( 'NONE', *, *, #16963, .T. ) ;
#12810 = CARTESIAN_POINT ( 'NONE',  ( 20.00000000000000000, -2.500000000000000444, -16.99999999999999645 ) ) ;
#12812 = CARTESIAN_POINT ( 'NONE',  ( 1.254255976357671720, -9.426444230097072108, 11.25336128106933664 ) ) ;
#12813 = DIRECTION ( 'NONE',  ( 0.000000000000000000, -0.8660254037844384856, 0.5000000000000004441 ) ) ;
#12814 = B_SPLINE_CURVE_WITH_KNOTS ( 'NONE', 3,
 ( #4830, #12090, #16583, #17925, #9028, #4636, #3478, #7901, #5959, #10460, #16297, #3666, #18105 ),
 .UNSPECIFIED., .F., .F.,
 ( 4, 3, 3, 3, 4 ),
 ( 3.144186300207962859E-18, 0.0002299780670421060105, 0.0004599561239687904998, 0.0006896788984287882803, 0.0009194956271626397379 ),
 .UNSPECIFIED. ) ;
#12815 = ORIENTED_EDGE ( 'NONE', *, *, #2804, .F. ) ;
#12816 = CARTESIAN_POINT ( 'NONE',  ( 0.3307726912345211323, -0.5948952607471654774, -13.74203354050372461 ) ) ;
#12817 = CARTESIAN_POINT ( 'NONE',  ( 0.3137051932979792457, 0.4596302728641686874, -13.73004976592201487 ) ) ;
#12818 = ORIENTED_EDGE ( 'NONE', *, *, #1914, .F. ) ;
#12819 = CARTESIAN_POINT ( 'NONE',  ( 2.636624412715138366, -11.10302021257964888, 11.60464335004044223 ) ) ;
#12820 = SURFACE_STYLE_FILL_AREA ( #2321 ) ;
#12821 = CARTESIAN_POINT ( 'NONE',  ( 0.000000000000000000, 0.000000000000000000, -3.000000000000000000 ) ) ;
#12822 = CARTESIAN_POINT ( 'NONE',  ( 0.3151926232592536792, -11.07013665200800645, 8.137833541809341042 ) ) ;
#12823 = CARTESIAN_POINT ( 'NONE',  ( 2.636624412714236865, 0.000000000000000000, 0.000000000000000000 ) ) ;
#12824 = EDGE_CURVE ( 'NONE', #9336, #5926, #5324, .T. ) ;
#12825 = ITEM_DEFINED_TRANSFORMATION ( 'NONE', 'NONE', #12127,  #2030 ) ;
#12826 = CARTESIAN_POINT ( 'NONE',  ( -114.9284586926032574, -81.60345299795268659, -93.42422730238307338 ) ) ;
#12827 = EDGE_CURVE ( 'NONE', #16571, #102, #2759, .T. ) ;
#12828 = CARTESIAN_POINT ( 'NONE',  ( 3.074695600507268978, -2.772091048739378394, 15.30693405987788935 ) ) ;
#12829 = CARTESIAN_POINT ( 'NONE',  ( 1.846138399168762101, -4.238866729160323032, -11.69739621335926394 ) ) ;
#12830 = CARTESIAN_POINT ( 'NONE',  ( 1.847034903785824023, 3.625649561595307269, 11.90269060117935496 ) ) ;
#12831 = CARTESIAN_POINT ( 'NONE',  ( 19.99999999999999645, 20.00000000000000000, 3.000000000000000000 ) ) ;
#12832 = ORIENTED_EDGE ( 'NONE', *, *, #9287, .T. ) ;
#12833 = CARTESIAN_POINT ( 'NONE',  ( 0.3145729642390365788, 10.93201268464384768, -8.321438378985135387 ) ) ;
#12834 = CARTESIAN_POINT ( 'NONE',  ( 16.56753206892534891, -0.001421777558676855365, -0.009389754735541546229 ) ) ;
#12835 = B_SPLINE_CURVE_WITH_KNOTS ( 'NONE', 3,
 ( #3039, #10231, #8887, #4597 ),
 .UNSPECIFIED., .F., .F.,
 ( 4, 4 ),
 ( 0.000000000000000000, 0.002004993803842297466 ),
 .UNSPECIFIED. ) ;
#12836 = ORIENTED_EDGE ( 'NONE', *, *, #4035, .T. ) ;
#12837 = ORIENTED_EDGE ( 'NONE', *, *, #1515, .T. ) ;
#12839 = CARTESIAN_POINT ( 'NONE',  ( -194.9999999999999716, -5.000000000000024869, -2.000000000000000000 ) ) ;
#12838 = AXIS2_PLACEMENT_3D ( 'NONE', #10494, #2917, #7254 ) ;
#12840 = ORIENTED_EDGE ( 'NONE', *, *, #922, .T. ) ;
#12841 = CARTESIAN_POINT ( 'NONE',  ( 0.3150690434770172521, -0.1531837610934980720, 13.73846430619029491 ) ) ;
#12842 = VERTEX_POINT ( 'NONE', #16456 ) ;
#12843 = DIRECTION ( 'NONE',  ( -1.000000000000000000, -0.000000000000000000, -0.000000000000000000 ) ) ;
#12844 = DIRECTION ( 'NONE',  ( 0.000000000000000000, -1.000000000000000000, 0.000000000000000000 ) ) ;
#12845 = FACE_BOUND ( 'NONE', #6094, .T. ) ;
#12846 = FACE_OUTER_BOUND ( 'NONE', #9863, .T. ) ;
#12847 = EDGE_CURVE ( 'NONE', #14456, #10910, #18632, .T. ) ;
#12848 = ADVANCED_FACE ( 'NONE', ( #9178 ), #6129, .F. ) ;
#12849 = DIRECTION ( 'NONE',  ( -0.000000000000000000, -0.000000000000000000, -1.000000000000000000 ) ) ;
#12850 = EDGE_CURVE ( 'NONE', #6105, #15002, #1243, .T. ) ;
#12851 = AXIS2_PLACEMENT_3D ( 'NONE', #15492, #5266, #8515 ) ;
#12852 = CARTESIAN_POINT ( 'NONE',  ( 0.3148208552358917611, -0.2299193288886511033, -13.73693263646119078 ) ) ;
#12853 = CARTESIAN_POINT ( 'NONE',  ( 0.3720661004400040439, -12.89739157014196635, 4.951033743989591507 ) ) ;
#12854 = DIRECTION ( 'NONE',  ( 0.7635533937278216055, -0.2197766120036547532, 0.6071939193889553943 ) ) ;
#12855 = VERTEX_POINT ( 'NONE', #10522 ) ;
#12856 =( BOUNDED_SURFACE ( )  B_SPLINE_SURFACE ( 3, 1, ( 
 ( #17617, #1750 ),
 ( #7596, #2779 ),
 ( #11976, #1463 ),
 ( #223, #16178 ) ),
 .UNSPECIFIED., .F., .F., .T. ) 
 B_SPLINE_SURFACE_WITH_KNOTS ( ( 4, 4 ),
 ( 2, 2 ),
 ( 0.000000000000000000, 1.000000000000000000 ),
 ( 0.000000000000000000, 1.000000000000000000 ),
 .UNSPECIFIED. ) 
 GEOMETRIC_REPRESENTATION_ITEM ( )  RATIONAL_B_SPLINE_SURFACE ( (
 ( 1.000000000000000000, 1.000000000000000000),
 ( 0.9933953342250438912, 0.8357391271907739227),
 ( 0.9933953342250438912, 0.8357391271907739227),
 ( 1.000000000000000000, 1.000000000000000000) ) ) 
 REPRESENTATION_ITEM ( '' )  SURFACE ( )  );
#12857 = EDGE_LOOP ( 'NONE', ( #6958, #10354, #4245, #10159 ) ) ;
#12858 = ORIENTED_EDGE ( 'NONE', *, *, #192, .F. ) ;
#12859 = ORIENTED_EDGE ( 'NONE', *, *, #3991, .F. ) ;
#12860 = CARTESIAN_POINT ( 'NONE',  ( 1.847380140988742925, 3.740232970470921625, -11.86779270755354432 ) ) ;
#12861 = B_SPLINE_CURVE_WITH_KNOTS ( 'NONE', 3,
 ( #10865, #2336, #906, #13721, #12557, #8180 ),
 .UNSPECIFIED., .F., .F.,
 ( 4, 2, 4 ),
 ( 1.084202172485504314E-19, 0.001657017934711308349, 0.003314035869422615830 ),
 .UNSPECIFIED. ) ;
#12862 = CARTESIAN_POINT ( 'NONE',  ( 0.3720661004400037664, -13.34435358167255181, 3.575426119359132571 ) ) ;
#12863 = CARTESIAN_POINT ( 'NONE',  ( 8.438534575730034959, -0.2320579683289648587, -6.862570336891078426 ) ) ;
#12864 = VERTEX_POINT ( 'NONE', #16357 ) ;
#12865 = DIRECTION ( 'NONE',  ( -1.000000000000000000, 0.000000000000000000, 0.000000000000000000 ) ) ;
#12866 = CARTESIAN_POINT ( 'NONE',  ( 0.000000000000000000, -1.732050807568877859, -1.752539433813135784E-17 ) ) ;
#12867 = CARTESIAN_POINT ( 'NONE',  ( 2.826946895708269736, 6.438259034076401655, -12.00000001686870732 ) ) ;
#12868 = DIRECTION ( 'NONE',  ( 0.7561779333270775005, -0.03481510524965699543, 0.6534392409364816467 ) ) ;
#12869 = FACE_OUTER_BOUND ( 'NONE', #7785, .T. ) ;
#12870 = CARTESIAN_POINT ( 'NONE',  ( 0.4862570985993252548, -12.97920246947875889, -5.003653737315625349 ) ) ;
#12871 = B_SPLINE_CURVE_WITH_KNOTS ( 'NONE', 3,
 ( #16763, #2057, #7900, #9409 ),
 .UNSPECIFIED., .F., .F.,
 ( 4, 4 ),
 ( 0.000000000000000000, 0.002004993803842607548 ),
 .UNSPECIFIED. ) ;
#12872 = CARTESIAN_POINT ( 'NONE',  ( 0.000000000000000000, 0.000000000000000000, 10.00000000000000000 ) ) ;
#12873 = EDGE_CURVE ( 'NONE', #5602, #12106, #10099, .T. ) ;
#12874 = CARTESIAN_POINT ( 'NONE',  ( 3.950837973638675393, -2.591948120961912849, 14.31366178983252446 ) ) ;
#12875 = ORIENTED_EDGE ( 'NONE', *, *, #4504, .T. ) ;
#12876 = EDGE_CURVE ( 'NONE', #8134, #6766, #8748, .T. ) ;
#12877 = VERTEX_POINT ( 'NONE', #12052 ) ;
#12878 = CARTESIAN_POINT ( 'NONE',  ( 0.3170788640506441158, -13.74111462631963576, 0.1533108587035682813 ) ) ;
#12879 = FACE_OUTER_BOUND ( 'NONE', #6116, .T. ) ;
#12880 = EDGE_LOOP ( 'NONE', ( #1429, #1828, #16159, #14850 ) ) ;
#12881 = CIRCLE ( 'NONE', #16565, 1.500000000000000000 ) ;
#12882 = CARTESIAN_POINT ( 'NONE',  ( 1.847034903785822690, -0.2299360331935046409, 12.44051878787773013 ) ) ;
#12883 = ADVANCED_FACE ( 'NONE', ( #10716 ), #7013, .F. ) ;
#12884 = ORIENTED_EDGE ( 'NONE', *, *, #566, .T. ) ;
#12885 = CARTESIAN_POINT ( 'NONE',  ( 0.3308579732647013438, -3.680601586799781000, -13.25341063505879546 ) ) ;
#12886 = CARTESIAN_POINT ( 'NONE',  ( 1.847034903785823579, -12.44051878787772836, -0.2299360331935480506 ) ) ;
#12887 = CARTESIAN_POINT ( 'NONE',  ( -30.00000000000000355, -12.50000000000000178, -0.5000000000000000000 ) ) ;
#12888 = CARTESIAN_POINT ( 'NONE',  ( 2.123976203522053297, 13.47898556379324297, -7.899625852120059299 ) ) ;
#12889 = VERTEX_POINT ( 'NONE', #13158 ) ;
#12890 = CARTESIAN_POINT ( 'NONE',  ( 2.353870697619111940, 6.980654702310842730, 10.90705766126222187 ) ) ;
#12891 = CIRCLE ( 'NONE', #9544, 2.750000000000000000 ) ;
#12892 = LINE ( 'NONE', #13180, #14013 ) ;
#12893 = LINE ( 'NONE', #18718, #17406 ) ;
#12894 = SHAPE_REPRESENTATION ( 'gear driver shaft', ( #2030 ), #4780 ) ;
#12895 =( BOUNDED_SURFACE ( )  B_SPLINE_SURFACE ( 3, 1, ( 
 ( #7771, #2125 ),
 ( #13687, #9099 ),
 ( #15017, #17898 ),
 ( #6428, #6140 ) ),
 .UNSPECIFIED., .F., .F., .T. ) 
 B_SPLINE_SURFACE_WITH_KNOTS ( ( 4, 4 ),
 ( 2, 2 ),
 ( 0.000000000000000000, 1.000000000000000000 ),
 ( 0.000000000000000000, 1.000000000000000000 ),
 .UNSPECIFIED. ) 
 GEOMETRIC_REPRESENTATION_ITEM ( )  RATIONAL_B_SPLINE_SURFACE ( (
 ( 1.000000000000000000, 1.000000000000000000),
 ( 0.9933953342250438912, 0.8357391271907739227),
 ( 0.9933953342250438912, 0.8357391271907739227),
 ( 1.000000000000000000, 1.000000000000000000) ) ) 
 REPRESENTATION_ITEM ( '' )  SURFACE ( )  );
#12896 = CARTESIAN_POINT ( 'NONE',  ( 0.3142014840576535795, -12.94260032291125562, -4.608051180497059640 ) ) ;
#12897 = CARTESIAN_POINT ( 'NONE',  ( 15.00000000000000711, -45.00000000000000000, 0.000000000000000000 ) ) ;
#12898 = APPLICATION_CONTEXT ( 'automotive_design' ) ;
#12899 = DIRECTION ( 'NONE',  ( 0.8370013143907355513, 0.4246593920385846599, -0.3450988270939222002 ) ) ;
#12900 = LINE ( 'NONE', #1533, #8058 ) ;
#12901 = ORIENTED_EDGE ( 'NONE', *, *, #16232, .F. ) ;
#12902 = B_SPLINE_CURVE_WITH_KNOTS ( 'NONE', 3,
 ( #11744, #5704, #14795, #7452 ),
 .UNSPECIFIED., .F., .F.,
 ( 4, 4 ),
 ( 2.851299179213411365E-16, 0.002004993803842618823 ),
 .UNSPECIFIED. ) ;
#12903 = EDGE_CURVE ( 'NONE', #2858, #14346, #4279, .T. ) ;
#12904 = DIRECTION ( 'NONE',  ( 0.000000000000000000, 1.000000000000000000, 0.000000000000000000 ) ) ;
#12906 = EDGE_LOOP ( 'NONE', ( #135, #7288, #18118, #9177 ) ) ;
#12905 = LINE ( 'NONE', #1154, #4804 ) ;
#12907 = CARTESIAN_POINT ( 'NONE',  ( 8.522092701127531811, -6.489356537178209372, 2.505958102592595882 ) ) ;
#12908 = PLANE ( 'NONE',  #16243 ) ;
#12909 = ORIENTED_EDGE ( 'NONE', *, *, #581, .T. ) ;
#12910 = CARTESIAN_POINT ( 'NONE',  ( 0.3137051932979775248, 3.805684345189972895, -13.20008686438101719 ) ) ;
#12911 = CARTESIAN_POINT ( 'NONE',  ( 0.3132642857406558456, 10.79548167658034608, 8.495623922778108295 ) ) ;
#12912 = ORIENTED_EDGE ( 'NONE', *, *, #17435, .T. ) ;
#12913 = CARTESIAN_POINT ( 'NONE',  ( 16.56872352241294521, -0.01033355228142500762, -0.001442253899401184716 ) ) ;
#12914 = LINE ( 'NONE', #17411, #17699 ) ;
#12915 = CARTESIAN_POINT ( 'NONE',  ( 0.3148208552358935375, -4.026279359288518656, 13.13564827777588029 ) ) ;
#12916 = CARTESIAN_POINT ( 'NONE',  ( 4.000000000000000888, 20.00000000000000000, 8.000000000000000000 ) ) ;
#12917 = CARTESIAN_POINT ( 'NONE',  ( 0.3058872367615226295, -13.72992299905059355, -0.6080468242582393046 ) ) ;
#12918 = B_SPLINE_CURVE_WITH_KNOTS ( 'NONE', 3,
 ( #13352, #8857, #9050, #559, #4464, #356 ),
 .UNSPECIFIED., .F., .F.,
 ( 4, 2, 4 ),
 ( 2.468197616305571356E-18, 0.0002017457492448094245, 0.0004034914984896164096 ),
 .UNSPECIFIED. ) ;
#12919 = AXIS2_PLACEMENT_3D ( 'NONE', #6372, #13521, #3585 ) ;
#12920 = EDGE_LOOP ( 'NONE', ( #18592, #9943 ) ) ;
#12921 = VECTOR ( 'NONE', #14581, 1000.000000000000000 ) ;
#12922 = DIRECTION ( 'NONE',  ( -1.000000000000000000, 0.000000000000000000, 0.000000000000000000 ) ) ;
#12923 = CARTESIAN_POINT ( 'NONE',  ( 1.846138399168762101, -6.971848976711082280, 10.30487220521567693 ) ) ;
#12924 = FACE_OUTER_BOUND ( 'NONE', #5800, .T. ) ;
#12925 = CARTESIAN_POINT ( 'NONE',  ( 16.56753206892534891, -0.009389754735541561842, 0.001421777558676752366 ) ) ;
#12926 = LINE ( 'NONE', #9694, #15767 ) ;
#12927 = VERTEX_POINT ( 'NONE', #14589 ) ;
#12928 = CARTESIAN_POINT ( 'NONE',  ( 3.950837973638668288, 0.000000000000000000, 0.000000000000000000 ) ) ;
#12929 = SURFACE_SIDE_STYLE ('',( #15607 ) ) ;
#12930 = ORIENTED_EDGE ( 'NONE', *, *, #160, .F. ) ;
#12931 = EDGE_CURVE ( 'NONE', #18033, #15020, #15900, .T. ) ;
#12932 = VERTEX_POINT ( 'NONE', #8663 ) ;
#12933 = CARTESIAN_POINT ( 'NONE',  ( 1.847426409206450959, -2.029922383240494730E-11, 12.44303504652081038 ) ) ;
#12934 = CIRCLE ( 'NONE', #5307, 5.000000000000000000 ) ;
#12935 = VECTOR ( 'NONE', #16329, 1000.000000000000114 ) ;
#12936 = ORIENTED_EDGE ( 'NONE', *, *, #428, .T. ) ;
#12937 = CARTESIAN_POINT ( 'NONE',  ( 0.3142014840576501378, -0.3830336514509840029, 13.73311050063163918 ) ) ;
#12938 = PRODUCT_DEFINITION_FORMATION_WITH_SPECIFIED_SOURCE ( 'ANY', '', #15013, .NOT_KNOWN. ) ;
#12939 = ORIENTED_EDGE ( 'NONE', *, *, #10209, .F. ) ;
#12940 = DIRECTION ( 'NONE',  ( -1.000000000000000000, 0.000000000000000000, 0.000000000000000000 ) ) ;
#12941 = CARTESIAN_POINT ( 'NONE',  ( 0.3137051932979757485, 12.91601973349276733, -4.679953077377353665 ) ) ;
#12942 = PLANE ( 'NONE',  #15120 ) ;
#12943 = LINE ( 'NONE', #7416, #3829 ) ;
#12944 = DIRECTION ( 'NONE',  ( -0.7561779333270775005, -0.1688126975276600938, 0.6322161072786937064 ) ) ;
#12945 = CARTESIAN_POINT ( 'NONE',  ( 8.438534575730034959, 5.415535776177522465, 4.221456476902686106 ) ) ;
#12946 = CARTESIAN_POINT ( 'NONE',  ( 2.747332970342022840, 2.409922051470906990, -16.17136872824896443 ) ) ;
#12947 = CARTESIAN_POINT ( 'NONE',  ( 16.57605080000000086, 4.769696007084728073, 1.500000000000000000 ) ) ;
#12948 = ORIENTED_EDGE ( 'NONE', *, *, #3109, .T. ) ;
#12949 = ORIENTED_EDGE ( 'NONE', *, *, #9989, .T. ) ;
#12950 = ORIENTED_EDGE ( 'NONE', *, *, #4931, .T. ) ;
#12951 = VERTEX_POINT ( 'NONE', #7637 ) ;
#12952 = ORIENTED_EDGE ( 'NONE', *, *, #5570, .F. ) ;
#12953 = VECTOR ( 'NONE', #1689, 1000.000000000000000 ) ;
#12954 = EDGE_CURVE ( 'NONE', #17449, #6674, #5751, .T. ) ;
#12955 = PLANE ( 'NONE',  #6258 ) ;
#12956 = CIRCLE ( 'NONE', #6268, 1.000000000000000000 ) ;
#12957 = CARTESIAN_POINT ( 'NONE',  ( 16.56753206892534891, -0.009389754735542259201, -0.001421777558675912110 ) ) ;
#12958 = VERTEX_POINT ( 'NONE', #8952 ) ;
#12959 = CARTESIAN_POINT ( 'NONE',  ( 25.00000000000000000, 2.499999999999998668, -17.00000000000000000 ) ) ;
#12960 = AXIS2_PLACEMENT_3D ( 'NONE', #9799, #5322, #18686 ) ;
#12961 = CARTESIAN_POINT ( 'NONE',  ( 8.438534575730034959, -6.598402093327893958, 1.899950616255162483 ) ) ;
#12962 = CARTESIAN_POINT ( 'NONE',  ( 5.682963807814618740, 7.499999999999998224, -12.81889723681830695 ) ) ;
#12963 = CARTESIAN_POINT ( 'NONE',  ( 0.4862570985993235340, -0.7479633556561480212, -13.89016912371018186 ) ) ;
#12964 = FACE_OUTER_BOUND ( 'NONE', #3214, .T. ) ;
#12965 = CARTESIAN_POINT ( 'NONE',  ( 1.846613052777651198, 4.166957398589849149, 11.72395935470500028 ) ) ;
#12966 = FACE_OUTER_BOUND ( 'NONE', #2003, .T. ) ;
#12967 =( BOUNDED_SURFACE ( )  B_SPLINE_SURFACE ( 3, 1, ( 
 ( #18777, #16978 ),
 ( #2801, #9791 ),
 ( #7130, #11528 ),
 ( #15622, #3887 ) ),
 .UNSPECIFIED., .F., .F., .T. ) 
 B_SPLINE_SURFACE_WITH_KNOTS ( ( 4, 4 ),
 ( 2, 2 ),
 ( 0.000000000000000000, 1.000000000000000000 ),
 ( 0.000000000000000000, 1.000000000000000000 ),
 .UNSPECIFIED. ) 
 GEOMETRIC_REPRESENTATION_ITEM ( )  RATIONAL_B_SPLINE_SURFACE ( (
 ( 1.000000000000000000, 1.000000000000000000),
 ( 0.9933953342250436691, 0.8357391271907733676),
 ( 0.9933953342250436691, 0.8357391271907733676),
 ( 1.000000000000000000, 1.000000000000000000) ) ) 
 REPRESENTATION_ITEM ( '' )  SURFACE ( )  );
#12968 = CARTESIAN_POINT ( 'NONE',  ( 15.00000000000000711, -19.99999999999999645, 8.000000000000000000 ) ) ;
#12969 = ORIENTED_EDGE ( 'NONE', *, *, #6980, .F. ) ;
#12970 = AXIS2_PLACEMENT_3D ( 'NONE', #8529, #9766, #18742 ) ;
#12971 = VECTOR ( 'NONE', #6781, 1000.000000000000000 ) ;
#12972 = ORIENTED_EDGE ( 'NONE', *, *, #7643, .T. ) ;
#12973 = ORIENTED_EDGE ( 'NONE', *, *, #5105, .F. ) ;
#12974 = ORIENTED_EDGE ( 'NONE', *, *, #10784, .T. ) ;
#12975 = DIRECTION ( 'NONE',  ( 0.000000000000000000, 0.000000000000000000, -1.000000000000000000 ) ) ;
#12976 = B_SPLINE_CURVE_WITH_KNOTS ( 'NONE', 3,
 ( #4063, #12662, #5305, #9787 ),
 .UNSPECIFIED., .F., .F.,
 ( 4, 4 ),
 ( 2.298835888684693015E-16, 0.002004993803842571552 ),
 .UNSPECIFIED. ) ;
#12977 = EDGE_CURVE ( 'NONE', #5607, #1182, #5992, .T. ) ;
#12978 = ORIENTED_EDGE ( 'NONE', *, *, #18076, .F. ) ;
#12979 = ADVANCED_FACE ( 'NONE', ( #10195 ), #15593, .F. ) ;
#12980 = CARTESIAN_POINT ( 'NONE',  ( 2.636624412716062071, -14.14563173255412742, -7.605649742760987486 ) ) ;
#12981 = CARTESIAN_POINT ( 'NONE',  ( 1.847168016377983335, 11.89018175117595177, 3.666915430942639720 ) ) ;
#12982 = CARTESIAN_POINT ( 'NONE',  ( 0.3058872367615230181, 7.578326039752771415, -11.46514199369349818 ) ) ;
#12983 = EDGE_LOOP ( 'NONE', ( #17213, #13498, #2402, #3440, #227 ) ) ;
#12984 = CARTESIAN_POINT ( 'NONE',  ( -1.127570259384925242E-14, -6.520075332560959849E-30, 26.00000000000000000 ) ) ;
#12985 = CARTESIAN_POINT ( 'NONE',  ( 1.846138399168762101, -10.30487220521565028, -6.971848976711123136 ) ) ;
#12986 = CIRCLE ( 'NONE', #16366, 4.750000000000000000 ) ;
#12987 = CARTESIAN_POINT ( 'NONE',  ( 2.002547531651519996, 4.532360870844494016, -11.75462648437097180 ) ) ;
#12988 = CARTESIAN_POINT ( 'NONE',  ( 0.3151930723728408879, -13.04315954105012310, -4.318364831037728280 ) ) ;
#12989 = CARTESIAN_POINT ( 'NONE',  ( 0.000000000000000000, 0.000000000000000000, 11.00000000000000000 ) ) ;
#12990 = CARTESIAN_POINT ( 'NONE',  ( 3.950837973638675393, -2.591948120961706792, -14.31366178983255466 ) ) ;
#12991 = CARTESIAN_POINT ( 'NONE',  ( 0.000000000000000000, 0.000000000000000000, 13.74999999999999822 ) ) ;
#12992 = DIRECTION ( 'NONE',  ( -1.000000000000000000, -0.000000000000000000, -0.000000000000000000 ) ) ;
#12993 = ORIENTED_EDGE ( 'NONE', *, *, #14954, .F. ) ;
#12994 = B_SPLINE_CURVE_WITH_KNOTS ( 'NONE', 3,
 ( #14488, #13151, #5590, #15731, #2723, #2632, #8479, #63, #11443, #17261, #14394, #17457, #8568 ),
 .UNSPECIFIED., .F., .F.,
 ( 4, 3, 3, 3, 4 ),
 ( 2.453269466693398698E-18, 0.0002299780670421020532, 0.0004599561239687888735, 0.0006896788984287890393, 0.0009194956271626411473 ),
 .UNSPECIFIED. ) ;
#12995 = CARTESIAN_POINT ( 'NONE',  ( 1.846138399168762101, 6.971848976711159551, -10.30487220521562541 ) ) ;
#12997 = ORIENTED_EDGE ( 'NONE', *, *, #3339, .T. ) ;
#12996 = CARTESIAN_POINT ( 'NONE',  ( 0.4754618798421167414, 3.583352865732670534, 13.45049478164061263 ) ) ;
#12998 = CARTESIAN_POINT ( 'NONE',  ( 0.3145729642390366343, 7.825496023201474749, -11.29233589755984113 ) ) ;
#12999 = AXIS2_PLACEMENT_3D ( 'NONE', #9783, #11145, #14006 ) ;
#13000 = CARTESIAN_POINT ( 'NONE',  ( 1.846138399168762101, -9.815003036200353748, -7.646096044340000120 ) ) ;
#13001 =( GEOMETRIC_REPRESENTATION_CONTEXT ( 3 ) GLOBAL_UNCERTAINTY_ASSIGNED_CONTEXT ( ( #10368 ) ) GLOBAL_UNIT_ASSIGNED_CONTEXT ( ( #6917, #3858, #18565 ) ) REPRESENTATION_CONTEXT ( 'NONE', 'WORKASPACE' ) );
#13002 = VERTEX_POINT ( 'NONE', #7346 ) ;
#13003 = CARTESIAN_POINT ( 'NONE',  ( 0.3132635586635977298, -0.5277914263192144961, -13.72732610560089128 ) ) ;
#13004 = CARTESIAN_POINT ( 'NONE',  ( 0.4754618798421171855, 13.89949764182682657, -0.7484603771384882309 ) ) ;
#13005 = EDGE_LOOP ( 'NONE', ( #14559, #16914, #17159, #11072 ) ) ;
#13006 = CARTESIAN_POINT ( 'NONE',  ( 1.846138399168762101, -6.971848976711082280, 10.30487220521567693 ) ) ;
#13007 = CARTESIAN_POINT ( 'NONE',  ( 1.977228804422057840, -3.321884655132009811, 15.04020501276143662 ) ) ;
#13008 = ADVANCED_FACE ( 'NONE', ( #69 ), #16162, .F. ) ;
#13009 = LINE ( 'NONE', #1067, #8514 ) ;
#13010 = CARTESIAN_POINT ( 'NONE',  ( 0.3151926232592480726, -0.07678256780548071980, -13.73922722301401578 ) ) ;
#13011 = CARTESIAN_POINT ( 'NONE',  ( 0.3720661004400037664, -13.79610186261029270, -0.7231997263366251039 ) ) ;
#13012 = VERTEX_POINT ( 'NONE', #1795 ) ;
#13013 = CONICAL_SURFACE ( 'NONE', #4790, 14.54644660717763927, 0.8559913436420816257 ) ;
#13014 = COLOUR_RGB ( '', 0.40784314, 0.44705882, 0.49803922) ;
#13015 = B_SPLINE_CURVE_WITH_KNOTS ( 'NONE', 3,
 ( #13960, #9285, #961, #3643, #3551, #7968 ),
 .UNSPECIFIED., .F., .F.,
 ( 4, 2, 4 ),
 ( 3.897476843869763523E-18, 0.0002017457492448077711, 0.0004034914984896116391 ),
 .UNSPECIFIED. ) ;
#13016 = VECTOR ( 'NONE', #4134, 1000.000000000000000 ) ;
#13017 =( NAMED_UNIT ( * ) PLANE_ANGLE_UNIT ( ) SI_UNIT ( $, .RADIAN. ) );
#13018 = CARTESIAN_POINT ( 'NONE',  ( 1.321128355694181398E-14, -8.013167318348349610, 25.01316734529530095 ) ) ;
#13019 = CARTESIAN_POINT ( 'NONE',  ( 2.747332970342022840, 16.17136872824898575, -2.409922051470736459 ) ) ;
#13020 = CARTESIAN_POINT ( 'NONE',  ( 16.56782317627811096, 0.006045301465876630996, 0.007739510688078455984 ) ) ;
#13021 = CARTESIAN_POINT ( 'NONE',  ( -61.35602477868047799, -15.00000000000000711, 6.000000000000000000 ) ) ;
#13022 = CARTESIAN_POINT ( 'NONE',  ( 0.3132642857406501835, 7.641821025099867271, 11.41580579227779779 ) ) ;
#13023 = AXIS2_PLACEMENT_3D ( 'NONE', #13100, #16358, #17791 ) ;
#13024 = ORIENTED_EDGE ( 'NONE', *, *, #9317, .F. ) ;
#13025 = CARTESIAN_POINT ( 'NONE',  ( 15.00000000000000711, -18.99999999999999645, 7.000000000000000000 ) ) ;
#13026 = CARTESIAN_POINT ( 'NONE',  ( 0.3095370825347224519, -11.38092634279633941, 7.700448427571837229 ) ) ;
#13027 = ORIENTED_EDGE ( 'NONE', *, *, #8387, .F. ) ;
#13028 = VECTOR ( 'NONE', #18679, 1000.000000000000000 ) ;
#13029 = ORIENTED_EDGE ( 'NONE', *, *, #5310, .T. ) ;
#13030 = DIRECTION ( 'NONE',  ( 0.000000000000000000, 0.000000000000000000, -1.000000000000000000 ) ) ;
#13031 = VERTEX_POINT ( 'NONE', #14497 ) ;
#13032 = CARTESIAN_POINT ( 'NONE',  ( 1.846138399168762101, -3.446241763652916124, -11.95493567637853971 ) ) ;
#13033 = EDGE_CURVE ( 'NONE', #6505, #10137, #9661, .T. ) ;
#13034 = ORIENTED_EDGE ( 'NONE', *, *, #13873, .F. ) ;
#13035 = ADVANCED_FACE ( 'NONE', ( #7250 ), #8859, .T. ) ;
#13036 = DIRECTION ( 'NONE',  ( -1.000000000000000000, 0.000000000000000000, -6.938893903907225419E-16 ) ) ;
#13037 = CARTESIAN_POINT ( 'NONE',  ( 0.3151928476913548605, 13.06671852871095574, -4.245853234426248513 ) ) ;
#13038 =( REPRESENTATION_RELATIONSHIP ('NONE','NONE', #5200, #8995 ) REPRESENTATION_RELATIONSHIP_WITH_TRANSFORMATION ( #17223 )SHAPE_REPRESENTATION_RELATIONSHIP( ) );
#13039 = DIRECTION ( 'NONE',  ( 0.000000000000000000, 0.000000000000000000, 1.000000000000000000 ) ) ;
#13040 = CARTESIAN_POINT ( 'NONE',  ( 0.8740764193771586310, 12.04241474978035420, -7.708542792189425619 ) ) ;
#13041 = SHAPE_REPRESENTATION_RELATIONSHIP ( 'NONE' , 'NONE' ,  #5797, #18114 ) ;
#13042 = CARTESIAN_POINT ( 'NONE',  ( 1.847426409206450959, 1.966388007708274189E-11, -12.44303504652081038 ) ) ;
#13043 = DIRECTION ( 'NONE',  ( -1.000000000000000000, -0.000000000000000000, -0.000000000000000000 ) ) ;
#13044 = CARTESIAN_POINT ( 'NONE',  ( 16.56753206892534891, 0.009389754735541551434, -0.001421777558676823056 ) ) ;
#13045 = CARTESIAN_POINT ( 'NONE',  ( 2.636624412715137922, -7.605649742761668719, 14.14563173255331741 ) ) ;
#13046 = EDGE_CURVE ( 'NONE', #18257, #10202, #8512, .T. ) ;
#13047 = ORIENTED_EDGE ( 'NONE', *, *, #3811, .F. ) ;
#13048 = UNCERTAINTY_MEASURE_WITH_UNIT (LENGTH_MEASURE( 1.000000000000000082E-05 ), #18467, 'distance_accuracy_value', 'NONE');
#13049 = ORIENTED_EDGE ( 'NONE', *, *, #5699, .F. ) ;
#13050 = CIRCLE ( 'NONE', #18848, 3.499999999999992895 ) ;
#13051 = VERTEX_POINT ( 'NONE', #14684 ) ;
#13052 = EDGE_LOOP ( 'NONE', ( #8545, #15213 ) ) ;
#13053 = ORIENTED_EDGE ( 'NONE', *, *, #3522, .T. ) ;
#13054 = LINE ( 'NONE', #5588, #16930 ) ;
#13055 = CARTESIAN_POINT ( 'NONE',  ( 2.636624412714763555, 6.973567714907159321, 14.46769361191226722 ) ) ;
#13056 = DIRECTION ( 'NONE',  ( -1.000000000000000000, 2.891205793294679805E-16, 0.000000000000000000 ) ) ;
#13057 = ORIENTED_EDGE ( 'NONE', *, *, #8590, .F. ) ;
#13058 = CARTESIAN_POINT ( 'NONE',  ( 2.636624412714763555, 6.973567714907159321, 14.46769361191226722 ) ) ;
#13059 = DIRECTION ( 'NONE',  ( -1.000000000000000000, -0.000000000000000000, -0.000000000000000000 ) ) ;
#13060 = CARTESIAN_POINT ( 'NONE',  ( 18.75000000000000000, 0.000000000000000000, 0.000000000000000000 ) ) ;
#13061 = DIRECTION ( 'NONE',  ( 0.000000000000000000, 0.000000000000000000, 1.000000000000000000 ) ) ;
#13062 = CARTESIAN_POINT ( 'NONE',  ( 1.254009781011994340, -1.011465182608154434, -14.64464726212624690 ) ) ;
#13063 = DIRECTION ( 'NONE',  ( 1.000000000000000000, -2.775557561562892929E-15, 0.000000000000000000 ) ) ;
#13064 = CARTESIAN_POINT ( 'NONE',  ( 1.918921323896210840, 9.738309537478938793, 7.860085869556105109 ) ) ;
#13065 = CARTESIAN_POINT ( 'NONE',  ( 8.438534575730034959, 6.862570336891075762, -0.2320579683290367456 ) ) ;
#13066 = FACE_OUTER_BOUND ( 'NONE', #12624, .T. ) ;
#13067 = ADVANCED_FACE ( 'NONE', ( #13251 ), #11642, .F. ) ;
#13068 = EDGE_LOOP ( 'NONE', ( #5374, #3085, #11437, #17353 ) ) ;
#13069 = B_SPLINE_CURVE_WITH_KNOTS ( 'NONE', 3,
 ( #1776, #8751, #14866, #1491 ),
 .UNSPECIFIED., .F., .F.,
 ( 4, 4 ),
 ( 0.000000000000000000, 0.002004993803842287058 ),
 .UNSPECIFIED. ) ;
#13070 = ORIENTED_EDGE ( 'NONE', *, *, #9024, .F. ) ;
#13071 = ORIENTED_EDGE ( 'NONE', *, *, #9289, .F. ) ;
#13072 = ORIENTED_EDGE ( 'NONE', *, *, #11297, .F. ) ;
#13073 = B_SPLINE_CURVE_WITH_KNOTS ( 'NONE', 3,
 ( #17852, #3405, #12018, #15346, #9437, #18224 ),
 .UNSPECIFIED., .F., .F.,
 ( 4, 2, 4 ),
 ( 2.710505431213761085E-19, 0.001657017934710631590, 0.003314035869421263179 ),
 .UNSPECIFIED. ) ;
#13074 = CARTESIAN_POINT ( 'NONE',  ( 2.002547531651519996, 12.57989064830759496, 0.6781519942172178350 ) ) ;
#13075 = ORIENTED_EDGE ( 'NONE', *, *, #1831, .F. ) ;
#13076 = CARTESIAN_POINT ( 'NONE',  ( -199.9999999999999716, 4.999999999999973355, 6.000000000000000000 ) ) ;
#13077 = B_SPLINE_CURVE_WITH_KNOTS ( 'NONE', 3,
 ( #1740, #13486, #6232, #10636 ),
 .UNSPECIFIED., .F., .F.,
 ( 4, 4 ),
 ( 1.330347433792404293E-17, 0.003005512676784847462 ),
 .UNSPECIFIED. ) ;
#13078 = DIRECTION ( 'NONE',  ( 0.000000000000000000, 0.000000000000000000, 1.000000000000000000 ) ) ;
#13079 = CARTESIAN_POINT ( 'NONE',  ( 3.950837973638675393, -10.51028938476210328, -10.05648675950137871 ) ) ;
#13080 = CARTESIAN_POINT ( 'NONE',  ( -194.9999999999999716, 9.999999999999973355, 11.00000000000000000 ) ) ;
#13081 = CONICAL_SURFACE ( 'NONE', #3313, 14.54644660717763927, 0.8559913436420816257 ) ;
#13082 = ORIENTED_EDGE ( 'NONE', *, *, #15084, .F. ) ;
#13083 = DIRECTION ( 'NONE',  ( -1.000000000000000000, 0.000000000000000000, 0.000000000000000000 ) ) ;
#13084 = DIRECTION ( 'NONE',  ( -0.000000000000000000, 0.000000000000000000, -1.000000000000000000 ) ) ;
#13085 = CARTESIAN_POINT ( 'NONE',  ( 0.3151926232592509591, -13.73922722301401400, 0.07678256780552859817 ) ) ;
#13086 = CARTESIAN_POINT ( 'NONE',  ( 0.3137051932979792457, -12.91601973349266963, -4.679953077377624560 ) ) ;
#13087 =( BOUNDED_SURFACE ( )  B_SPLINE_SURFACE ( 3, 1, ( 
 ( #919, #18398 ),
 ( #11156, #14098 ),
 ( #7034, #15717 ),
 ( #9708, #3883 ) ),
 .UNSPECIFIED., .F., .F., .T. ) 
 B_SPLINE_SURFACE_WITH_KNOTS ( ( 4, 4 ),
 ( 2, 2 ),
 ( 0.000000000000000000, 1.000000000000000000 ),
 ( 0.000000000000000000, 1.000000000000000000 ),
 .UNSPECIFIED. ) 
 GEOMETRIC_REPRESENTATION_ITEM ( )  RATIONAL_B_SPLINE_SURFACE ( (
 ( 1.000000000000000000, 1.000000000000000000),
 ( 0.9593108457356467333, 0.9995965569486454649),
 ( 0.9593108457356467333, 0.9995965569486454649),
 ( 1.000000000000000000, 1.000000000000000000) ) ) 
 REPRESENTATION_ITEM ( '' )  SURFACE ( )  );
#13088 = CARTESIAN_POINT ( 'NONE',  ( 1.847168016377983335, 11.89018175117595177, 3.666915430942639720 ) ) ;
#13089 = CARTESIAN_POINT ( 'NONE',  ( 2.636624412715137922, -14.46769361191291559, 6.973567714907789927 ) ) ;
#13090 = EDGE_CURVE ( 'NONE', #11279, #14839, #15069, .T. ) ;
#13091 = CARTESIAN_POINT ( 'NONE',  ( 158.9967805326548671, -32.56920798809784401, 61.71538810391422913 ) ) ;
#13092 = CYLINDRICAL_SURFACE ( 'NONE', #1009, 2.100000000000000977 ) ;
#13093 = EDGE_CURVE ( 'NONE', #2050, #7024, #13073, .T. ) ;
#13094 = EDGE_CURVE ( 'NONE', #14429, #13318, #12257, .T. ) ;
#13095 = ORIENTED_EDGE ( 'NONE', *, *, #3384, .F. ) ;
#13096 = ORIENTED_EDGE ( 'NONE', *, *, #6275, .F. ) ;
#13097 = AXIS2_PLACEMENT_3D ( 'NONE', #12610, #9657, #6429 ) ;
#13098 = CARTESIAN_POINT ( 'NONE',  ( 0.4862570985993252548, -12.97920246947875889, -5.003653737315625349 ) ) ;
#13099 = CIRCLE ( 'NONE', #7008, 2.055000000000000160 ) ;
#13101 = ORIENTED_EDGE ( 'NONE', *, *, #15062, .T. ) ;
#13100 = CARTESIAN_POINT ( 'NONE',  ( 3.950837973638668288, 0.000000000000000000, 0.000000000000000000 ) ) ;
#13102 = CARTESIAN_POINT ( 'NONE',  ( 0.3720661004400040439, 3.575426119359372823, -13.34435358167249142 ) ) ;
#13103 = DIRECTION ( 'NONE',  ( 0.000000000000000000, 0.000000000000000000, 1.000000000000000000 ) ) ;
#13104 = EDGE_LOOP ( 'NONE', ( #6062, #552, #3113, #2605 ) ) ;
#13105 = CARTESIAN_POINT ( 'NONE',  ( 16.56872352241294521, -0.004907101719995745834, -0.009207754980064182873 ) ) ;
#13106 = CARTESIAN_POINT ( 'NONE',  ( 1.560000000000000053, 0.000000000000000000, 2.999999999999998668 ) ) ;
#13107 = EDGE_CURVE ( 'NONE', #6766, #666, #6187, .T. ) ;
#13108 = VERTEX_POINT ( 'NONE', #6387 ) ;
#13109 = CARTESIAN_POINT ( 'NONE',  ( 16.56753206892534891, 0.006760771273035115839, -0.006669401563385219701 ) ) ;
#13110 = CARTESIAN_POINT ( 'NONE',  ( 2.320521194582657376, -3.126729093671833937, 15.43440938317077915 ) ) ;
#13111 = CARTESIAN_POINT ( 'NONE',  ( 0.4385251269669978580, 3.577373010348713134, 13.39302348765809825 ) ) ;
#13112 = CARTESIAN_POINT ( 'NONE',  ( 0.3137051932979792457, -13.73004976592202375, 0.4596302728639276580 ) ) ;
#13113 = CONTEXT_DEPENDENT_SHAPE_REPRESENTATION ( #6213, #2922 ) ;
#13114 =( NAMED_UNIT ( * ) SI_UNIT ( $, .STERADIAN. ) SOLID_ANGLE_UNIT ( ) );
#13115 = CARTESIAN_POINT ( 'NONE',  ( 3.512766787570772653, -2.682019731918489303, 14.81029789862156143 ) ) ;
#13116 = CARTESIAN_POINT ( 'NONE',  ( -194.9999999999999716, 14.99999999999997513, 3.000000000000002665 ) ) ;
#13117 = CARTESIAN_POINT ( 'NONE',  ( 16.58200780006414732, -0.008650561019685578876, 0.007066318000004673597 ) ) ;
#13118 = CARTESIAN_POINT ( 'NONE',  ( 0.3132635586635995617, 11.41586812343490109, 7.641727604903931770 ) ) ;
#13119 = CARTESIAN_POINT ( 'NONE',  ( 1.861628059977341154, -12.44564375541077084, -0.5393144007391572625 ) ) ;
#13120 = EDGE_CURVE ( 'NONE', #2733, #10257, #10689, .T. ) ;
#13121 = ORIENTED_EDGE ( 'NONE', *, *, #18614, .T. ) ;
#13122 = CARTESIAN_POINT ( 'NONE',  ( 1.560000000000000053, 1.732050807568878747, 7.017607234860990640E-28 ) ) ;
#13123 =( BOUNDED_SURFACE ( )  B_SPLINE_SURFACE ( 3, 1, ( 
 ( #12685, #2109 ),
 ( #12414, #7949 ),
 ( #9460, #13755 ),
 ( #9541, #3624 ) ),
 .UNSPECIFIED., .F., .F., .T. ) 
 B_SPLINE_SURFACE_WITH_KNOTS ( ( 4, 4 ),
 ( 2, 2 ),
 ( 0.000000000000000000, 1.000000000000000000 ),
 ( 0.000000000000000000, 1.000000000000000000 ),
 .UNSPECIFIED. ) 
 GEOMETRIC_REPRESENTATION_ITEM ( )  RATIONAL_B_SPLINE_SURFACE ( (
 ( 1.000000000000000000, 1.000000000000000000),
 ( 0.7792777138730160313, 0.9689936506012927220),
 ( 0.7792777138730160313, 0.9689936506012927220),
 ( 1.000000000000000000, 1.000000000000000000) ) ) 
 REPRESENTATION_ITEM ( '' )  SURFACE ( )  );
#13124 = CARTESIAN_POINT ( 'NONE',  ( 1.560000000000000053, -0.8660254037844384856, 1.500000000000000000 ) ) ;
#13125 = ORIENTED_EDGE ( 'NONE', *, *, #15086, .F. ) ;
#13126 = ORIENTED_EDGE ( 'NONE', *, *, #5186, .F. ) ;
#13127 = CARTESIAN_POINT ( 'NONE',  ( 2.747332970342022840, -16.17136872824897154, -2.409922051470850146 ) ) ;
#13128 = ORIENTED_EDGE ( 'NONE', *, *, #9873, .T. ) ;
#13129 = CARTESIAN_POINT ( 'NONE',  ( 2.179449471770337432, -4.500000000000000000, 0.000000000000000000 ) ) ;
#13130 = EDGE_LOOP ( 'NONE', ( #9282, #14, #1608, #7375 ) ) ;
#13131 = EDGE_CURVE ( 'NONE', #15452, #11172, #4180, .T. ) ;
#13132 = DIRECTION ( 'NONE',  ( -0.000000000000000000, -0.5000000000000004441, 0.8660254037844383745 ) ) ;
#13133 = CARTESIAN_POINT ( 'NONE',  ( 0.4754618798421167414, -3.583352865732579051, -13.45049478164063217 ) ) ;
#13134 = CARTESIAN_POINT ( 'NONE',  ( -2.179449471770337432, -4.500000000000000000, -3.000000000000000000 ) ) ;
#13135 = PLANE ( 'NONE',  #9958 ) ;
#13136 = CARTESIAN_POINT ( 'NONE',  ( 0.3145729642390363567, -7.825496023201391260, 11.29233589755989797 ) ) ;
#13137 = CARTESIAN_POINT ( 'NONE',  ( 0.000000000000000000, 0.000000000000000000, 0.000000000000000000 ) ) ;
#13138 = DIRECTION ( 'NONE',  ( 0.000000000000000000, 0.000000000000000000, 1.000000000000000000 ) ) ;
#13139 = CARTESIAN_POINT ( 'NONE',  ( 2.002547531651519996, -3.242439124566736997, 12.17374746633577232 ) ) ;
#13140 = CARTESIAN_POINT ( 'NONE',  ( 16.57778382496167424, 0.01018821665058777630, -0.01092721432668997822 ) ) ;
#13141 = CARTESIAN_POINT ( 'NONE',  ( 16.57778382496167424, 0.002851818597093999999, -0.01466529584256785410 ) ) ;
#13142 = ORIENTED_EDGE ( 'NONE', *, *, #951, .T. ) ;
#13143 = DIRECTION ( 'NONE',  ( 0.000000000000000000, -1.000000000000000000, 0.000000000000000000 ) ) ;
#13144 = ORIENTED_EDGE ( 'NONE', *, *, #14077, .F. ) ;
#13145 = VERTEX_POINT ( 'NONE', #18042 ) ;
#13146 = ORIENTED_EDGE ( 'NONE', *, *, #5514, .T. ) ;
#13147 = ORIENTED_EDGE ( 'NONE', *, *, #1710, .T. ) ;
#13148 = ADVANCED_FACE ( 'NONE', ( #13820 ), #13593, .F. ) ;
#13149 = CARTESIAN_POINT ( 'NONE',  ( 1.861628059977342931, -12.00316790821103652, 3.332996951203584413 ) ) ;
#13150 = CARTESIAN_POINT ( 'NONE',  ( 1.959283090834856633, -0.6676170829051342182, -12.53713130127478692 ) ) ;
#13151 = CARTESIAN_POINT ( 'NONE',  ( 0.3142014840576500267, 8.382000553815611710, -10.88517824918533883 ) ) ;
#13152 = ORIENTED_EDGE ( 'NONE', *, *, #16854, .F. ) ;
#13153 = FACE_OUTER_BOUND ( 'NONE', #7917, .T. ) ;
#13154 = EDGE_CURVE ( 'NONE', #14694, #12032, #8101, .T. ) ;
#13155 = CARTESIAN_POINT ( 'NONE',  ( 3.074695600507182824, 6.754521329825023734, -14.01296402267889007 ) ) ;
#13156 = CIRCLE ( 'NONE', #12838, 0.5000000000000004441 ) ;
#13157 = CARTESIAN_POINT ( 'NONE',  ( 2.002547531651519996, -3.242439124566736997, 12.17374746633577232 ) ) ;
#13158 = CARTESIAN_POINT ( 'NONE',  ( 3.950837973638675393, 14.31366178983257242, -2.591948120961654833 ) ) ;
#13159 = DIRECTION ( 'NONE',  ( 0.000000000000000000, 0.000000000000000000, 1.000000000000000000 ) ) ;
#13160 = CARTESIAN_POINT ( 'NONE',  ( 1.847247051441594401, 0.1676840720647037319, -12.44188156437793680 ) ) ;
#13161 = CARTESIAN_POINT ( 'NONE',  ( 1.977228804422057840, -3.321884655132009811, 15.04020501276143662 ) ) ;
#13162 = CARTESIAN_POINT ( 'NONE',  ( 0.3151930723728431083, -11.07033375389125673, -8.137566970826481949 ) ) ;
#13163 = CARTESIAN_POINT ( 'NONE',  ( 0.000000000000000000, 0.000000000000000000, 0.000000000000000000 ) ) ;
#13164 = EDGE_LOOP ( 'NONE', ( #4956, #9777, #9602, #8946 ) ) ;
#13165 = PRODUCT_DEFINITION_SHAPE ( 'NONE', 'NONE',  #18912 ) ;
#13166 = ORIENTED_EDGE ( 'NONE', *, *, #17327, .T. ) ;
#13167 = ORIENTED_EDGE ( 'NONE', *, *, #2706, .T. ) ;
#13168 = EDGE_LOOP ( 'NONE', ( #3980, #13813, #9333, #15187 ) ) ;
#13169 = CARTESIAN_POINT ( 'NONE',  ( 16.56753206892534891, 0.006760771273035115839, -0.006669401563385219701 ) ) ;
#13170 = EDGE_CURVE ( 'NONE', #4291, #12792, #16426, .T. ) ;
#13171 = VERTEX_POINT ( 'NONE', #647 ) ;
#13172 = CARTESIAN_POINT ( 'NONE',  ( -199.9999999999999716, -5.000000000000024869, 3.000000000000000000 ) ) ;
#13173 = CARTESIAN_POINT ( 'NONE',  ( 2.369999999999999662, 0.000000000000000000, 4.750000000000000000 ) ) ;
#13174 = FACE_OUTER_BOUND ( 'NONE', #15758, .T. ) ;
#13175 = AXIS2_PLACEMENT_3D ( 'NONE', #13457, #6199, #17869 ) ;
#13176 = CARTESIAN_POINT ( 'NONE',  ( 1.847426409206450959, 1.966388007708274189E-11, -12.44303504652081038 ) ) ;
#13177 = ORIENTED_EDGE ( 'NONE', *, *, #14767, .F. ) ;
#13178 = PLANE ( 'NONE',  #10533 ) ;
#13179 = ADVANCED_FACE ( 'NONE', ( #360 ), #9344, .T. ) ;
#13180 = CARTESIAN_POINT ( 'NONE',  ( 2.426025403784448642, 2.655529440325959183E-32, -2.168404344971008868E-16 ) ) ;
#13181 = FACE_OUTER_BOUND ( 'NONE', #6852, .T. ) ;
#13182 = DIRECTION ( 'NONE',  ( -0.000000000000000000, 0.000000000000000000, -1.000000000000000000 ) ) ;
#13183 = CARTESIAN_POINT ( 'NONE',  ( 0.3151928476913583022, 13.06684726503526761, 4.245457024760265874 ) ) ;
#13184 = ORIENTED_EDGE ( 'NONE', *, *, #4942, .T. ) ;
#13185 = CIRCLE ( 'NONE', #8027, 16.06066017081991149 ) ;
#13186 = CARTESIAN_POINT ( 'NONE',  ( 1.847247051441592181, 7.448813758297314180, -9.967131402978116839 ) ) ;
#13188 = VERTEX_POINT ( 'NONE', #1895 ) ;
#13187 = DIRECTION ( 'NONE',  ( -1.000000000000000000, 0.000000000000000000, 0.000000000000000000 ) ) ;
#13189 = CARTESIAN_POINT ( 'NONE',  ( 0.3142014840576500267, 8.382000553815611710, -10.88517824918533883 ) ) ;
#13190 = DIRECTION ( 'NONE',  ( -0.000000000000000000, -0.000000000000000000, 1.000000000000000000 ) ) ;
#13191 = EDGE_LOOP ( 'NONE', ( #1759, #8973, #8940, #1724 ) ) ;
#13192 = CARTESIAN_POINT ( 'NONE',  ( 0.4384471787762841966, -0.7363690479465361260, -13.84291427302852817 ) ) ;
#13193 = UNCERTAINTY_MEASURE_WITH_UNIT (LENGTH_MEASURE( 1.000000000000000082E-05 ), #14378, 'distance_accuracy_value', 'NONE');
#13194 = DIRECTION ( 'NONE',  ( 0.000000000000000000, 0.000000000000000000, 1.000000000000000000 ) ) ;
#13195 =( BOUNDED_SURFACE ( )  B_SPLINE_SURFACE ( 3, 1, ( 
 ( #4707, #6234 ),
 ( #17900, #118 ),
 ( #16273, #17806 ),
 ( #11779, #10537 ) ),
 .UNSPECIFIED., .F., .F., .T. ) 
 B_SPLINE_SURFACE_WITH_KNOTS ( ( 4, 4 ),
 ( 2, 2 ),
 ( 0.000000000000000000, 1.000000000000000000 ),
 ( 0.000000000000000000, 1.000000000000000000 ),
 .UNSPECIFIED. ) 
 GEOMETRIC_REPRESENTATION_ITEM ( )  RATIONAL_B_SPLINE_SURFACE ( (
 ( 1.000000000000000000, 1.000000000000000000),
 ( 0.7792777138730158093, 0.9689936506012928330),
 ( 0.7792777138730158093, 0.9689936506012928330),
 ( 1.000000000000000000, 1.000000000000000000) ) ) 
 REPRESENTATION_ITEM ( '' )  SURFACE ( )  );
#13196 = VERTEX_POINT ( 'NONE', #4855 ) ;
#13197 = FACE_OUTER_BOUND ( 'NONE', #13164, .T. ) ;
#13198 = ADVANCED_FACE ( 'NONE', ( #12121 ), #4003, .T. ) ;
#13199 = EDGE_CURVE ( 'NONE', #16036, #12529, #18759, .T. ) ;
#13200 = CARTESIAN_POINT ( 'NONE',  ( -5.000000000000000000, 6.123233995736766282E-16, 0.000000000000000000 ) ) ;
#13201 = B_SPLINE_CURVE_WITH_KNOTS ( 'NONE', 3,
 ( #9833, #11380, #5447, #15664 ),
 .UNSPECIFIED., .F., .F.,
 ( 4, 4 ),
 ( 3.750785467376078809E-16, 0.002004993803842428438 ),
 .UNSPECIFIED. ) ;
#13202 = DIRECTION ( 'NONE',  ( -1.000000000000000000, -0.000000000000000000, -0.000000000000000000 ) ) ;
#13203 = DIRECTION ( 'NONE',  ( 0.000000000000000000, -0.000000000000000000, 1.000000000000000000 ) ) ;
#13204 = VECTOR ( 'NONE', #12944, 1000.000000000000114 ) ;
#13205 =( NAMED_UNIT ( * ) PLANE_ANGLE_UNIT ( ) SI_UNIT ( $, .RADIAN. ) );
#13206 = FACE_OUTER_BOUND ( 'NONE', #884, .T. ) ;
#13207 = FACE_OUTER_BOUND ( 'NONE', #15778, .T. ) ;
#13208 = CARTESIAN_POINT ( 'NONE',  ( 0.4862570985993235340, 11.67702470553376060, -7.559321496869298329 ) ) ;
#13209 = CARTESIAN_POINT ( 'NONE',  ( 16.56872352241294521, -0.004564908236400030961, 0.009382111268607351909 ) ) ;
#13210 = EDGE_LOOP ( 'NONE', ( #657, #11600 ) ) ;
#13211 = CARTESIAN_POINT ( 'NONE',  ( 0.3151926232592475174, -8.013596737356467159, 11.16039997398650918 ) ) ;
#13212 = CARTESIAN_POINT ( 'NONE',  ( 16.56753206892534891, 0.006669401563384923931, -0.006760771273036191367 ) ) ;
#13213 = VERTEX_POINT ( 'NONE', #3810 ) ;
#13214 = EDGE_LOOP ( 'NONE', ( #7141, #13579, #15918 ) ) ;
#13215 = CARTESIAN_POINT ( 'NONE',  ( 16.56679352167444819, 0.006618561353599204840, -0.006526964904752983153 ) ) ;
#13216 = ORIENTED_EDGE ( 'NONE', *, *, #15004, .F. ) ;
#13217 = DIRECTION ( 'NONE',  ( 0.000000000000000000, 0.000000000000000000, -1.000000000000000000 ) ) ;
#13218 = ORIENTED_EDGE ( 'NONE', *, *, #7703, .F. ) ;
#13219 = EDGE_CURVE ( 'NONE', #13213, #16036, #17430, .T. ) ;
#13220 = AXIS2_PLACEMENT_3D ( 'NONE', #10373, #8844, #16203 ) ;
#13221 = EDGE_CURVE ( 'NONE', #13922, #12855, #83, .T. ) ;
#13222 = EDGE_CURVE ( 'NONE', #4747, #4298, #2460, .T. ) ;
#13223 = CARTESIAN_POINT ( 'NONE',  ( 0.3132635586635977298, -0.5277914263192144961, -13.72732610560089128 ) ) ;
#13224 = B_SPLINE_CURVE_WITH_KNOTS ( 'NONE', 3,
 ( #14734, #17322, #16278, #14452 ),
 .UNSPECIFIED., .F., .F.,
 ( 4, 4 ),
 ( 0.000000000000000000, 0.002004993803842618390 ),
 .UNSPECIFIED. ) ;
#13225 = CARTESIAN_POINT ( 'NONE',  ( 0.4754618798421171855, 8.775436892861110394, 10.80499583390516172 ) ) ;
#13226 = DIRECTION ( 'NONE',  ( -0.5052478564545411777, -0.8629742774544855166, 0.000000000000000000 ) ) ;
#13227 = CARTESIAN_POINT ( 'NONE',  ( 2.636624412716902288, 7.605649742760546950, -14.14563173255513995 ) ) ;
#13228 = UNCERTAINTY_MEASURE_WITH_UNIT (LENGTH_MEASURE( 1.000000000000000082E-05 ), #17202, 'distance_accuracy_value', 'NONE');
#13229 = DIRECTION ( 'NONE',  ( 0.000000000000000000, -0.8660254037844384856, -0.5000000000000004441 ) ) ;
#13230 = CARTESIAN_POINT ( 'NONE',  ( 3.950837973638676281, -14.41405733518059229, -1.958075594453940971 ) ) ;
#13231 = CARTESIAN_POINT ( 'NONE',  ( 16.58200780006414732, -0.006043560077721775101, 0.009393638146078504489 ) ) ;
#13232 = CARTESIAN_POINT ( 'NONE',  ( 0.3939822652208120890, -10.75310269629515325, -8.678192463540291612 ) ) ;
#13233 = DIRECTION ( 'NONE',  ( -0.000000000000000000, -1.000000000000000000, -0.000000000000000000 ) ) ;
#13234 = CARTESIAN_POINT ( 'NONE',  ( 2.747332970342022840, -14.63517873738941866, -7.289199830147261139 ) ) ;
#13235 = VECTOR ( 'NONE', #1236, 1000.000000000000000 ) ;
#13236 = B_SPLINE_CURVE_WITH_KNOTS ( 'NONE', 3,
 ( #15905, #14466, #1090, #17438, #11332, #14565 ),
 .UNSPECIFIED., .F., .F.,
 ( 4, 2, 4 ),
 ( 2.790109556687801058E-18, 0.0002017457492448093974, 0.0004034914984896159759 ),
 .UNSPECIFIED. ) ;
#13237 = CARTESIAN_POINT ( 'NONE',  ( 0.3170788640506440603, 13.11595226728163510, -4.100430649997826471 ) ) ;
#13238 = CARTESIAN_POINT ( 'NONE',  ( 2.320521194582656932, -15.64520804578280888, 1.795798718313643683 ) ) ;
#13239 = ORIENTED_EDGE ( 'NONE', *, *, #3588, .T. ) ;
#13240 = ORIENTED_EDGE ( 'NONE', *, *, #318, .T. ) ;
#13241 = EDGE_LOOP ( 'NONE', ( #4671, #3728, #8594, #12183 ) ) ;
#13242 = ORIENTED_EDGE ( 'NONE', *, *, #15062, .F. ) ;
#13243 = CARTESIAN_POINT ( 'NONE',  ( 3.950837973638676281, 6.316429227969464932, 13.10350451991842569 ) ) ;
#13244 = DIRECTION ( 'NONE',  ( -0.000000000000000000, 1.000000000000000000, -0.000000000000000000 ) ) ;
#13245 = DIRECTION ( 'NONE',  ( 0.000000000000000000, 0.000000000000000000, 1.000000000000000000 ) ) ;
#13246 = ORIENTED_EDGE ( 'NONE', *, *, #11389, .F. ) ;
#13247 = CARTESIAN_POINT ( 'NONE',  ( -66.35602477868047799, 14.99999999999997513, 5.999999999999999112 ) ) ;
#13248 = CARTESIAN_POINT ( 'NONE',  ( 1.846138399168762101, -12.43476674860266229, -0.4167076046096845898 ) ) ;
#13249 = CONICAL_SURFACE ( 'NONE', #11728, 14.54644660717763927, 0.8559913436420816257 ) ;
#13250 = EDGE_CURVE ( 'NONE', #10871, #18854, #3257, .T. ) ;
#13251 = FACE_OUTER_BOUND ( 'NONE', #7720, .T. ) ;
#13252 = CARTESIAN_POINT ( 'NONE',  ( 3.950837973638675393, 14.31366178983257242, -2.591948120961654833 ) ) ;
#13253 = CARTESIAN_POINT ( 'NONE',  ( 0.000000000000000000, -0.8660254037844384856, 1.500000000000000000 ) ) ;
#13254 = CARTESIAN_POINT ( 'NONE',  ( 2.636624412716062071, -11.10302021258080352, -11.60464335004061454 ) ) ;
#13255 = CARTESIAN_POINT ( 'NONE',  ( 15.00000000000000711, -19.99999999999999645, 3.000000000000000000 ) ) ;
#13256 = CARTESIAN_POINT ( 'NONE',  ( 0.3142014840576502488, -7.762239086932773091, -11.33546131209471142 ) ) ;
#13257 = VERTEX_POINT ( 'NONE', #2280 ) ;
#13258 = B_SPLINE_CURVE_WITH_KNOTS ( 'NONE', 3,
 ( #1006, #11250, #6845, #9984, #7035, #17069, #12852, #2711, #3884, #11339 ),
 .UNSPECIFIED., .F., .F.,
 ( 4, 3, 3, 4 ),
 ( 0.0004597478348665241538, 0.0004599561239687906082, 0.0006896788984287882803, 0.0009194956271626397379 ),
 .UNSPECIFIED. ) ;
#13259 = VERTEX_POINT ( 'NONE', #8130 ) ;
#13260 = ORIENTED_EDGE ( 'NONE', *, *, #8760, .T. ) ;
#13261 = EDGE_CURVE ( 'NONE', #1036, #13957, #10093, .T. ) ;
#13262 = VERTEX_POINT ( 'NONE', #12506 ) ;
#13263 = CARTESIAN_POINT ( 'NONE',  ( 0.3058872367615230181, -3.664492643742856881, 13.24582953854924128 ) ) ;
#13264 = ORIENTED_EDGE ( 'NONE', *, *, #17693, .T. ) ;
#13265 = DIRECTION ( 'NONE',  ( -0.000000000000000000, -1.000000000000000000, -0.000000000000000000 ) ) ;
#13266 = CARTESIAN_POINT ( 'NONE',  ( 0.3095370825347224519, -13.20347358821911854, -3.806662003783552350 ) ) ;
#13267 = PRODUCT_RELATED_PRODUCT_CATEGORY ( 'part', '', ( #4477 ) ) ;
#13268 = FACE_OUTER_BOUND ( 'NONE', #14411, .T. ) ;
#13269 = EDGE_CURVE ( 'NONE', #15874, #15040, #10405, .T. ) ;
#13270 = DIRECTION ( 'NONE',  ( 0.7635533937278216055, -0.02138673900302784023, 0.6453904417649385383 ) ) ;
#13271 = ORIENTED_EDGE ( 'NONE', *, *, #7420, .T. ) ;
#13272 = CARTESIAN_POINT ( 'NONE',  ( 1.846822687350026193, -4.121816957446279517, 11.74004266906802663 ) ) ;
#13273 = EDGE_CURVE ( 'NONE', #4376, #6482, #9194, .T. ) ;
#13274 = DIRECTION ( 'NONE',  ( -0.000000000000000000, 0.5000000000000004441, 0.8660254037844383745 ) ) ;
#13275 = EDGE_CURVE ( 'NONE', #996, #4997, #9196, .T. ) ;
#13276 = B_SPLINE_CURVE_WITH_KNOTS ( 'NONE', 3,
 ( #9571, #4024, #15772, #8518, #16262, #5824 ),
 .UNSPECIFIED., .F., .F.,
 ( 4, 2, 4 ),
 ( 8.673617379884035472E-19, 0.001500839035891552223, 0.003001678071783103578 ),
 .UNSPECIFIED. ) ;
#13277 = DIRECTION ( 'NONE',  ( -1.000000000000000000, 0.000000000000000000, 0.000000000000000000 ) ) ;
#13278 = VECTOR ( 'NONE', #8078, 1000.000000000000000 ) ;
#13279 = AXIS2_PLACEMENT_3D ( 'NONE', #7709, #9750, #12094 ) ;
#13280 = AXIS2_PLACEMENT_3D ( 'NONE', #7460, #186, #14608 ) ;
#13281 = CARTESIAN_POINT ( 'NONE',  ( 0.3095370825347224519, 4.681152801286340370, -12.91933430393602933 ) ) ;
#13282 = EDGE_LOOP ( 'NONE', ( #18212, #7546, #12007, #868 ) ) ;
#13283 = CARTESIAN_POINT ( 'NONE',  ( 1.254255976357644409, -12.44256109021810097, 7.789651112956895496 ) ) ;
#13285 = ORIENTED_EDGE ( 'NONE', *, *, #11491, .F. ) ;
#13284 = CARTESIAN_POINT ( 'NONE',  ( 1.847426409206449405, 0.01438352405959898543, -12.44303504652077841 ) ) ;
#13286 = CARTESIAN_POINT ( 'NONE',  ( 1.562796894703937678, 0.000000000000000000, 0.000000000000000000 ) ) ;
#13287 = EDGE_CURVE ( 'NONE', #15356, #5087, #763, .T. ) ;
#13288 = CARTESIAN_POINT ( 'NONE',  ( 16.56679352167444819, -0.006618561353599251677, 0.006526964904752932846 ) ) ;
#13289 = EDGE_LOOP ( 'NONE', ( #15915, #10938, #2828, #15250 ) ) ;
#13290 = ADVANCED_FACE ( 'NONE', ( #12243 ), #8221, .T. ) ;
#13291 = CARTESIAN_POINT ( 'NONE',  ( 2.636624412714237309, 14.14563173255211126, 7.605649742762011556 ) ) ;
#13292 = CIRCLE ( 'NONE', #14208, 5.000000000000000888 ) ;
#13293 = CARTESIAN_POINT ( 'NONE',  ( 5.308815406012384663, -7.500000000000255795, -12.96907596528278184 ) ) ;
#13294 = CONICAL_SURFACE ( 'NONE', #2302, 12.15840553252917289, 0.7853981625000049371 ) ;
#13295 = EDGE_LOOP ( 'NONE', ( #11933, #18060, #18878, #5327 ) ) ;
#13296 = CARTESIAN_POINT ( 'NONE',  ( 16.56679352167444819, 0.004277682826582259769, -0.008252760440870513317 ) ) ;
#13297 = B_SPLINE_CURVE_WITH_KNOTS ( 'NONE', 3,
 ( #10061, #11785, #6148, #7396, #4618, #4329 ),
 .UNSPECIFIED., .F., .F.,
 ( 4, 2, 4 ),
 ( 5.421010862427522170E-19, 0.0001825746017570577750, 0.0003651492035141150078 ),
 .UNSPECIFIED. ) ;
#13298 =( NAMED_UNIT ( * ) PLANE_ANGLE_UNIT ( ) SI_UNIT ( $, .RADIAN. ) );
#13299 = CARTESIAN_POINT ( 'NONE',  ( 0.3132642857406504611, -7.641821025099783782, -11.41580579227785464 ) ) ;
#13300 = DIRECTION ( 'NONE',  ( 0.000000000000000000, 1.000000000000000000, 0.000000000000000000 ) ) ;
#13301 = ORIENTED_EDGE ( 'NONE', *, *, #962, .F. ) ;
#13302 =( LENGTH_UNIT ( ) NAMED_UNIT ( * ) SI_UNIT ( .MILLI., .METRE. ) );
#13303 = CARTESIAN_POINT ( 'NONE',  ( 1.560000000000000053, -1.732050807568877859, -1.752539433813135784E-17 ) ) ;
#13304 = CARTESIAN_POINT ( 'NONE',  ( 0.000000000000000000, 0.000000000000000000, 7.000000000000000000 ) ) ;
#13305 = VECTOR ( 'NONE', #18218, 1000.000000000000000 ) ;
#13306 = CARTESIAN_POINT ( 'NONE',  ( 2.123976203522053741, -15.26039569100257509, -3.347755036806064677 ) ) ;
#13307 = CARTESIAN_POINT ( 'NONE',  ( 2.697797270744668019, 11.26906156738836984, -7.053988368581739721 ) ) ;
#13308 = FACE_OUTER_BOUND ( 'NONE', #1172, .T. ) ;
#13309 = EDGE_CURVE ( 'NONE', #16119, #17964, #11216, .T. ) ;
#13310 = VERTEX_POINT ( 'NONE', #15100 ) ;
#13311 = CARTESIAN_POINT ( 'NONE',  ( 16.57210152137263393, 0.01361613799508855013, 0.005118120558001428358 ) ) ;
#13312 = CARTESIAN_POINT ( 'NONE',  ( -5.000000000000000000, 0.000000000000000000, 8.000000000000000000 ) ) ;
#13313 = VERTEX_POINT ( 'NONE', #2018 ) ;
#13314 = ORIENTED_EDGE ( 'NONE', *, *, #10100, .T. ) ;
#13315 = CARTESIAN_POINT ( 'NONE',  ( 0.3151928476913523069, 11.11514699826562946, -8.075884471919630769 ) ) ;
#13316 = VERTEX_POINT ( 'NONE', #4972 ) ;
#13317 = DIRECTION ( 'NONE',  ( 0.000000000000000000, 0.000000000000000000, 1.000000000000000000 ) ) ;
#13318 = VERTEX_POINT ( 'NONE', #18423 ) ;
#13319 = CARTESIAN_POINT ( 'NONE',  ( 0.3720661004400037664, 13.79610186261029625, 0.7231997263365286255 ) ) ;
#13320 = CARTESIAN_POINT ( 'NONE',  ( 3.950837973638668288, 0.000000000000000000, 0.000000000000000000 ) ) ;
#13321 = B_SPLINE_CURVE_WITH_KNOTS ( 'NONE', 3,
 ( #888, #17123, #12542, #9679, #2406, #8258 ),
 .UNSPECIFIED., .F., .F.,
 ( 4, 2, 4 ),
 ( 5.421010862427522170E-19, 0.0001825746017570583442, 0.0003651492035141161462 ),
 .UNSPECIFIED. ) ;
#13322 = CARTESIAN_POINT ( 'NONE',  ( 0.3137051932979757485, 13.73004976592202020, -0.4596302728640235258 ) ) ;
#13323 = DIRECTION ( 'NONE',  ( 0.000000000000000000, 0.000000000000000000, -1.000000000000000000 ) ) ;
#13324 = PRODUCT_DEFINITION_SHAPE ( 'NONE', 'NONE',  #10229 ) ;
#13325 = DIRECTION ( 'NONE',  ( 0.000000000000000000, 0.000000000000000000, -1.000000000000000000 ) ) ;
#13326 = CARTESIAN_POINT ( 'NONE',  ( 8.522092701127531811, 6.489356537178190720, 2.505958102592644288 ) ) ;
#13327 = FILL_AREA_STYLE_COLOUR ( '', #15149 ) ;
#13328 = DIRECTION ( 'NONE',  ( -0.000000000000000000, 1.000000000000000000, -0.000000000000000000 ) ) ;
#13329 = CYLINDRICAL_SURFACE ( 'NONE', #2371, 5.000000000000000888 ) ;
#13330 = VECTOR ( 'NONE', #13187, 1000.000000000000000 ) ;
#13331 = CARTESIAN_POINT ( 'NONE',  ( 8.522092701127531811, -5.397361180353110299, -4.388629235579637466 ) ) ;
#13332 = AXIS2_PLACEMENT_3D ( 'NONE', #1698, #467, #7545 ) ;
#13333 = CARTESIAN_POINT ( 'NONE',  ( 0.3148213771069373057, 13.73693585713733967, 0.2297580318215192152 ) ) ;
#13334 = EDGE_CURVE ( 'NONE', #14355, #14209, #6761, .T. ) ;
#13335 = AXIS2_PLACEMENT_3D ( 'NONE', #229, #9016, #17816 ) ;
#13336 = ADVANCED_FACE ( 'NONE', ( #9911 ), #11549, .F. ) ;
#13337 = EDGE_CURVE ( 'NONE', #13901, #3568, #3667, .T. ) ;
#13338 = CARTESIAN_POINT ( 'NONE',  ( 1.846822687350018866, -11.92063725419901843, 3.566003975885642774 ) ) ;
#13339 = CARTESIAN_POINT ( 'NONE',  ( 16.56679352167444819, 0.009170718284672540327, 0.001518074900130682347 ) ) ;
#13340 = ORIENTED_EDGE ( 'NONE', *, *, #13269, .T. ) ;
#13341 = AXIS2_PLACEMENT_3D ( 'NONE', #3827, #9655, #5073 ) ;
#13342 = ORIENTED_EDGE ( 'NONE', *, *, #4635, .T. ) ;
#13343 = VERTEX_POINT ( 'NONE', #18798 ) ;
#13344 = VERTEX_POINT ( 'NONE', #8394 ) ;
#13345 = DIRECTION ( 'NONE',  ( 1.000000000000000000, 0.000000000000000000, 0.000000000000000000 ) ) ;
#13346 = AXIS2_PLACEMENT_3D ( 'NONE', #4551, #11907, #16310 ) ;
#13347 = CARTESIAN_POINT ( 'NONE',  ( 1.499999999999999112, 4.769696007084728073, 7.000000000000000000 ) ) ;
#13348 = CARTESIAN_POINT ( 'NONE',  ( 2.002547531651519996, -11.75462648437098601, -4.532360870844453160 ) ) ;
#13349 = VERTEX_POINT ( 'NONE', #5600 ) ;
#13350 = DIRECTION ( 'NONE',  ( -0.000000000000000000, -1.000000000000000000, -0.000000000000000000 ) ) ;
#13351 = AXIS2_PLACEMENT_3D ( 'NONE', #12174, #18186, #5085 ) ;
#13352 = CARTESIAN_POINT ( 'NONE',  ( 0.3137051932979757485, -11.37800749014125223, -7.698472063774596030 ) ) ;
#13353 = CARTESIAN_POINT ( 'NONE',  ( 1.321128355694181398E-14, -8.013167318348353163, 25.01316734529530095 ) ) ;
#13354 = CARTESIAN_POINT ( 'NONE',  ( 0.000000000000000000, -18.99999999999999645, 7.000000000000000000 ) ) ;
#13355 = CARTESIAN_POINT ( 'NONE',  ( 0.3151926232592457966, 8.137833541809381899, 11.07013665200797625 ) ) ;
#13356 = CARTESIAN_POINT ( 'NONE',  ( 3.950837973638676281, 13.10350451991840615, 6.316429227969512894 ) ) ;
#13357 = LINE ( 'NONE', #174, #12935 ) ;
#13358 = CARTESIAN_POINT ( 'NONE',  ( 2.636624412716902288, 7.605649742760546950, -14.14563173255513995 ) ) ;
#13359 = LINE ( 'NONE', #7646, #2635 ) ;
#13360 = VECTOR ( 'NONE', #2434, 1000.000000000000227 ) ;
#13361 = VERTEX_POINT ( 'NONE', #14039 ) ;
#13362 = VERTEX_POINT ( 'NONE', #2731 ) ;
#13363 = EDGE_LOOP ( 'NONE', ( #17569, #7872, #3559, #18577 ) ) ;
#13364 = ADVANCED_FACE ( 'NONE', ( #12783 ), #5057, .F. ) ;
#13365 = ORIENTED_EDGE ( 'NONE', *, *, #13633, .F. ) ;
#13366 = CARTESIAN_POINT ( 'NONE',  ( 1.846138399168762101, -11.95493567637848109, -3.446241763653124401 ) ) ;
#13367 = ORIENTED_EDGE ( 'NONE', *, *, #1315, .F. ) ;
#13368 = CARTESIAN_POINT ( 'NONE',  ( 0.4384471787762819206, -11.63197976518323173, -7.540925784514680430 ) ) ;
#13369 = DIRECTION ( 'NONE',  ( 1.000000000000000000, 0.000000000000000000, 0.000000000000000000 ) ) ;
#13370 = FACE_OUTER_BOUND ( 'NONE', #9371, .T. ) ;
#13371 = CARTESIAN_POINT ( 'NONE',  ( 3.950837973638675393, 10.51028938476217967, 10.05648675950130233 ) ) ;
#13372 = ORIENTED_EDGE ( 'NONE', *, *, #14597, .F. ) ;
#13373 = CARTESIAN_POINT ( 'NONE',  ( 1.088636994872527408, 7.500000000000000000, -14.58255216580684177 ) ) ;
#13374 = EDGE_CURVE ( 'NONE', #16292, #18099, #18278, .T. ) ;
#13375 = CIRCLE ( 'NONE', #7592, 4.750000000000000000 ) ;
#13376 = CARTESIAN_POINT ( 'NONE',  ( 1.959212340397946450, 11.71715421693498449, 4.509090217468559203 ) ) ;
#13377 = ORIENTED_EDGE ( 'NONE', *, *, #4828, .F. ) ;
#13378 = CARTESIAN_POINT ( 'NONE',  ( 2.123976203522053297, 15.54801196254786966, 1.531817366691807125 ) ) ;
#13379 = CARTESIAN_POINT ( 'NONE',  ( 3.664313757352975376, -14.16986885736091395, -1.627055439596424513 ) ) ;
#13380 = AXIS2_PLACEMENT_3D ( 'NONE', #14847, #2047, #17918 ) ;
#13381 = ORIENTED_EDGE ( 'NONE', *, *, #17544, .T. ) ;
#13382 = ADVANCED_FACE ( 'NONE', ( #17091 ), #11338, .T. ) ;
#13383 = CARTESIAN_POINT ( 'NONE',  ( 1.254009781011619307, -11.25324419414205224, 9.426200207651413976 ) ) ;
#13385 = EDGE_LOOP ( 'NONE', ( #16945, #6194, #7693, #10656 ) ) ;
#13384 = CARTESIAN_POINT ( 'NONE',  ( 1.847247051441594401, 0.1676840720647037319, -12.44188156437793680 ) ) ;
#13386 = FACE_OUTER_BOUND ( 'NONE', #8877, .T. ) ;
#13387 = ADVANCED_FACE ( 'NONE', ( #8491 ), #15538, .F. ) ;
#13388 = ADVANCED_FACE ( 'NONE', ( #12966 ), #8578, .T. ) ;
#13389 = DIRECTION ( 'NONE',  ( -1.000000000000000000, -0.000000000000000000, -0.000000000000000000 ) ) ;
#13390 = ORIENTED_EDGE ( 'NONE', *, *, #5118, .F. ) ;
#13391 = CARTESIAN_POINT ( 'NONE',  ( 6.500132120881376707, -2.599948583552213144, -12.00000000000000000 ) ) ;
#13392 = ORIENTED_EDGE ( 'NONE', *, *, #15042, .F. ) ;
#13393 = CARTESIAN_POINT ( 'NONE',  ( 1.846955891736119293, 3.593597880662512623, -11.91257079808164576 ) ) ;
#13394 = DIRECTION ( 'NONE',  ( -0.7561779333270775005, 0.4122479608995705536, 0.5081796452863259761 ) ) ;
#13395 = CARTESIAN_POINT ( 'NONE',  ( 0.4862570985993235340, -10.79774104611379215, 8.769551628660700260 ) ) ;
#13396 = CARTESIAN_POINT ( 'NONE',  ( 2.636624412715384391, -11.60464335004044223, -11.10302021258006278 ) ) ;
#13397 = EDGE_CURVE ( 'NONE', #14839, #12951, #9811, .T. ) ;
#13398 = ORIENTED_EDGE ( 'NONE', *, *, #6574, .F. ) ;
#13399 = AXIS2_PLACEMENT_3D ( 'NONE', #7077, #3924, #11566 ) ;
#13400 = CARTESIAN_POINT ( 'NONE',  ( 1.847461586945732703, -10.04711372545050097, 7.341074796295904648 ) ) ;
#13401 = CARTESIAN_POINT ( 'NONE',  ( 0.3151928476913548050, 11.11539186930587242, 8.075547435846990751 ) ) ;
#13402 = CARTESIAN_POINT ( 'NONE',  ( 16.56753206892534891, -0.001549402974393209202, 0.009369540855502124857 ) ) ;
#13403 = DIRECTION ( 'NONE',  ( -1.000000000000000000, -0.000000000000000000, -0.000000000000000000 ) ) ;
#13404 = DIRECTION ( 'NONE',  ( -0.7071067811865474617, 8.659560562354932858E-17, -0.7071067811865474617 ) ) ;
#13405 =( REPRESENTATION_RELATIONSHIP ('NONE','NONE', #5200, #16816 ) REPRESENTATION_RELATIONSHIP_WITH_TRANSFORMATION ( #4415 )SHAPE_REPRESENTATION_RELATIONSHIP( ) );
#13406 = VERTEX_POINT ( 'NONE', #1216 ) ;
#13407 = CARTESIAN_POINT ( 'NONE',  ( 0.3151928476913592458, -4.245457024760312947, 13.06684726503524807 ) ) ;
#13408 = CARTESIAN_POINT ( 'NONE',  ( 16.56679352167444819, -0.001390132774595520624, -0.009190982326619362083 ) ) ;
#13409 = ORIENTED_EDGE ( 'NONE', *, *, #18195, .T. ) ;
#13410 = ORIENTED_EDGE ( 'NONE', *, *, #16604, .F. ) ;
#13411 = CARTESIAN_POINT ( 'NONE',  ( 0.3151930723728382788, 11.16020735774779027, -8.013866567350774517 ) ) ;
#13412 = CIRCLE ( 'NONE', #7635, 5.000000000000004441 ) ;
#13413 = EDGE_LOOP ( 'NONE', ( #4978, #4332, #15827 ) ) ;
#13414 = PLANE ( 'NONE',  #1290 ) ;
#13415 = VECTOR ( 'NONE', #14881, 1000.000000000000000 ) ;
#13416 = MECHANICAL_DESIGN_GEOMETRIC_PRESENTATION_REPRESENTATION (  '', ( #13725 ), #3646 ) ;
#13417 = EDGE_LOOP ( 'NONE', ( #7337, #10452, #6151, #8257, #15379 ) ) ;
#13418 = ADVANCED_FACE ( 'NONE', ( #1126 ), #11451, .T. ) ;
#13419 = CARTESIAN_POINT ( 'NONE',  ( 2.636624412714237309, 15.91454522070173638, -2.161493821596664144 ) ) ;
#13420 = DIRECTION ( 'NONE',  ( -1.000000000000000000, 0.000000000000000000, 0.000000000000000000 ) ) ;
#13421 = EDGE_CURVE ( 'NONE', #8935, #10941, #8669, .T. ) ;
#13422 = CARTESIAN_POINT ( 'NONE',  ( 1.560000000000000053, 0.000000000000000000, 0.000000000000000000 ) ) ;
#13423 = DIRECTION ( 'NONE',  ( -1.000000000000000000, -0.000000000000000000, -0.000000000000000000 ) ) ;
#13424 = SURFACE_SIDE_STYLE ('',( #5865 ) ) ;
#13425 = CARTESIAN_POINT ( 'NONE',  ( 1.846138399168762101, 0.4167076046095548603, 12.43476674860266762 ) ) ;
#13426 = CARTESIAN_POINT ( 'NONE',  ( 2.002547531651519996, 3.242439124566649511, 12.17374746633579541 ) ) ;
#13427 = ORIENTED_EDGE ( 'NONE', *, *, #16542, .T. ) ;
#13428 = CARTESIAN_POINT ( 'NONE',  ( 1.846138399168762101, 6.971848976711011225, 10.30487220521572667 ) ) ;
#13429 = CARTESIAN_POINT ( 'NONE',  ( -66.35602477868049220, 14.99999999999997513, -153.7432847437423789 ) ) ;
#13430 = DIRECTION ( 'NONE',  ( 0.000000000000000000, -0.000000000000000000, 1.000000000000000000 ) ) ;
#13431 = DIRECTION ( 'NONE',  ( 0.000000000000000000, 0.000000000000000000, 1.000000000000000000 ) ) ;
#13432 = ORIENTED_EDGE ( 'NONE', *, *, #13965, .T. ) ;
#13433 = ORIENTED_EDGE ( 'NONE', *, *, #15898, .T. ) ;
#13434 = VERTEX_POINT ( 'NONE', #14501 ) ;
#13435 = ORIENTED_EDGE ( 'NONE', *, *, #15956, .F. ) ;
#13436 = CARTESIAN_POINT ( 'NONE',  ( -61.35602477868047799, 9.999999999999973355, -153.7432847437423789 ) ) ;
#13437 = LINE ( 'NONE', #17752, #6270 ) ;
#13438 = CARTESIAN_POINT ( 'NONE',  ( 2.002547531651519996, 0.6781519942173496185, -12.57989064830758785 ) ) ;
#13439 = CARTESIAN_POINT ( 'NONE',  ( 0.3137051932979792457, 13.73004976592202198, 0.4596302728640249136 ) ) ;
#13440 = AXIS2_PLACEMENT_3D ( 'NONE', #17314, #2861, #17 ) ;
#13441 = ADVANCED_FACE ( 'NONE', ( #14886 ), #11632, .T. ) ;
#13442 = EDGE_CURVE ( 'NONE', #1858, #799, #4360, .T. ) ;
#13443 = CARTESIAN_POINT ( 'NONE',  ( 3.950837973638668288, 0.000000000000000000, 0.000000000000000000 ) ) ;
#13444 = EDGE_CURVE ( 'NONE', #7533, #11395, #10729, .T. ) ;
#13445 = B_SPLINE_CURVE_WITH_KNOTS ( 'NONE', 3,
 ( #12091, #12192, #7509, #16298, #18018, #13419 ),
 .UNSPECIFIED., .F., .F.,
 ( 4, 2, 4 ),
 ( 0.000000000000000000, 0.001657017934709842290, 0.003314035869419685448 ),
 .UNSPECIFIED. ) ;
#13446 = CARTESIAN_POINT ( 'NONE',  ( 16.56822296793089322, 0.006547366384936635295, 0.007741272030791194678 ) ) ;
#13447 = CARTESIAN_POINT ( 'NONE',  ( 3.512766787570761107, 14.91422000116819468, -2.025881399556438200 ) ) ;
#13448 = CARTESIAN_POINT ( 'NONE',  ( 0.3148208552358926493, 8.260375059853341639, 10.97826876274314856 ) ) ;
#13449 = CARTESIAN_POINT ( 'NONE',  ( 1.560000000000000053, 0.000000000000000000, -1.499999999999999556 ) ) ;
#13450 = CARTESIAN_POINT ( 'NONE',  ( 3.950837973638675393, 14.31366178983257242, -2.591948120961654833 ) ) ;
#13451 = DIRECTION ( 'NONE',  ( -1.000000000000000000, -0.000000000000000000, -0.000000000000000000 ) ) ;
#13452 = CARTESIAN_POINT ( 'NONE',  ( 0.3151926232592475174, 4.172630140040981317, -13.09050869763088443 ) ) ;
#13453 = ORIENTED_EDGE ( 'NONE', *, *, #2994, .F. ) ;
#13454 = ORIENTED_EDGE ( 'NONE', *, *, #10894, .F. ) ;
#13455 = VERTEX_POINT ( 'NONE', #4761 ) ;
#13456 = ORIENTED_EDGE ( 'NONE', *, *, #10294, .F. ) ;
#13457 = CARTESIAN_POINT ( 'NONE',  ( -30.00000000000000355, -12.50000000000000178, 6.500000000000000888 ) ) ;
#13458 = CARTESIAN_POINT ( 'NONE',  ( 3.950837973638675393, -10.51028938476210328, -10.05648675950137871 ) ) ;
#13459 = AXIS2_PLACEMENT_3D ( 'NONE', #7730, #16522, #9244 ) ;
#13460 = CARTESIAN_POINT ( 'NONE',  ( -30.00000000000000711, 20.00000000000000000, 3.000000000000000000 ) ) ;
#13461 = DIRECTION ( 'NONE',  ( -0.000000000000000000, -0.000000000000000000, 1.000000000000000000 ) ) ;
#13462 = CYLINDRICAL_SURFACE ( 'NONE', #3841, 5.000000000000000000 ) ;
#13463 = EDGE_CURVE ( 'NONE', #16462, #10980, #13156, .T. ) ;
#13464 = VERTEX_POINT ( 'NONE', #13255 ) ;
#13465 = CARTESIAN_POINT ( 'NONE',  ( 0.4862570985993235340, -0.7479633556563419772, 13.89016912371017121 ) ) ;
#13466 = CARTESIAN_POINT ( 'NONE',  ( 16.56753206892534891, 0.006760771273036174887, 0.006669401563384942146 ) ) ;
#13467 = DIRECTION ( 'NONE',  ( 0.000000000000000000, 0.000000000000000000, -1.000000000000000000 ) ) ;
#13468 = CARTESIAN_POINT ( 'NONE',  ( 1.560000000000000053, 1.732050807568878747, 7.017607234860990640E-28 ) ) ;
#13469 = EDGE_CURVE ( 'NONE', #6435, #18680, #8958, .T. ) ;
#13470 = DIRECTION ( 'NONE',  ( -0.000000000000000000, -0.000000000000000000, 1.000000000000000000 ) ) ;
#13471 = CARTESIAN_POINT ( 'NONE',  ( 0.3145734862173258373, 12.96846406299306587, 4.535879238194977070 ) ) ;
#13472 = EDGE_CURVE ( 'NONE', #14717, #9296, #16029, .T. ) ;
#13473 = CARTESIAN_POINT ( 'NONE',  ( -199.9999999999999716, 4.999999999999974243, 5.999999999999999112 ) ) ;
#13474 = ORIENTED_EDGE ( 'NONE', *, *, #3133, .T. ) ;
#13475 = CIRCLE ( 'NONE', #10420, 14.54644660717763927 ) ;
#13476 = CARTESIAN_POINT ( 'NONE',  ( 1.562796894703937678, 0.000000000000000000, 0.000000000000000000 ) ) ;
#13478 = VERTEX_POINT ( 'NONE', #5892 ) ;
#13477 = CARTESIAN_POINT ( 'NONE',  ( 2.320521194582183977, 6.542541239684722676, 14.32454473829914399 ) ) ;
#13479 = CARTESIAN_POINT ( 'NONE',  ( 0.3137051932979792457, 11.37800749014131263, 7.698472063774513430 ) ) ;
#13480 = CARTESIAN_POINT ( 'NONE',  ( 1.136782529653004747, -45.00000000000000000, 6.000000000000000000 ) ) ;
#13481 = EDGE_LOOP ( 'NONE', ( #704, #15408, #9018, #17721 ) ) ;
#13482 = DIRECTION ( 'NONE',  ( -0.7635533937278214944, -0.3966532189476559833, -0.5095610256143900951 ) ) ;
#13483 = CARTESIAN_POINT ( 'NONE',  ( 4.294575106067288317, -7.500000000000266454, -13.17881115347054788 ) ) ;
#13484 = ORIENTED_EDGE ( 'NONE', *, *, #14122, .F. ) ;
#13485 = DIRECTION ( 'NONE',  ( 0.7561779333270775005, 0.5491072561318364187, -0.3559159372837296664 ) ) ;
#13486 = CARTESIAN_POINT ( 'NONE',  ( 3.377929128793393687, 1.296196549818942501, 13.92579934231096317 ) ) ;
#13487 = CARTESIAN_POINT ( 'NONE',  ( 0.4862570985993235340, -7.559321496869339185, -11.67702470553373750 ) ) ;
#13488 = LINE ( 'NONE', #14924, #7192 ) ;
#13489 = EDGE_CURVE ( 'NONE', #14463, #18838, #1600, .T. ) ;
#13490 = EDGE_CURVE ( 'NONE', #15958, #13528, #16213, .T. ) ;
#13491 = ORIENTED_EDGE ( 'NONE', *, *, #5107, .F. ) ;
#13492 = CIRCLE ( 'NONE', #11065, 16.06066017081991149 ) ;
#13493 = CARTESIAN_POINT ( 'NONE',  ( -0.2192422490275049152, -45.00000000000000000, 6.000000000000000000 ) ) ;
#13494 = DIRECTION ( 'NONE',  ( 1.000000000000000000, 0.000000000000000000, 0.000000000000000000 ) ) ;
#13495 = B_SPLINE_CURVE_WITH_KNOTS ( 'NONE', 3,
 ( #934, #11171, #9902, #18413, #18600, #1569, #17083, #139, #8738, #3899, #8835, #11080, #14657 ),
 .UNSPECIFIED., .F., .F.,
 ( 4, 3, 3, 3, 4 ),
 ( 3.127317220692750759E-18, 0.0002299804304191498290, 0.0004599608082120264186, 0.0006467586077648000654, 0.0008336169836825974228 ),
 .UNSPECIFIED. ) ;
#13496 = DIRECTION ( 'NONE',  ( 0.000000000000000000, 0.000000000000000000, 1.000000000000000000 ) ) ;
#13498 = ORIENTED_EDGE ( 'NONE', *, *, #18211, .T. ) ;
#13497 = CARTESIAN_POINT ( 'NONE',  ( 0.3170788640506440603, -8.200855617524609897, 11.02668139258439162 ) ) ;
#13499 = CARTESIAN_POINT ( 'NONE',  ( 2.705023505549862151, 8.489131503859777439, 10.24007717649583782 ) ) ;
#13500 = EDGE_LOOP ( 'NONE', ( #13034, #236, #18763, #470, #8112, #10791, #3072, #12399, #7256, #8248, #13744, #16827, #16290, #15253, #8914, #5952, #2210, #3793, #18637, #2626, #12768, #638, #17481, #8987, #14947, #13547, #11165, #15111, #8184, #17681, #16362, #1188, #12176, #10912, #8698, #5739, #18213, #4945, #12427, #13707, #2140, #16479, #16185, #10183, #11343, #5410, #13314, #14537, #11259, #10872, #14873, #8652, #10327, #9323, #10549, #5274, #3943, #12354, #1104, #7628, #10423, #3024, #8202, #13096 ) ) ;
#13501 = DIRECTION ( 'NONE',  ( -0.7635533937278214944, -0.6071939193889592801, 0.2197766120036439286 ) ) ;
#13502 = CARTESIAN_POINT ( 'NONE',  ( 3.512766787570759774, -13.55823433651952925, 6.535475144496928124 ) ) ;
#13503 = ORIENTED_EDGE ( 'NONE', *, *, #7158, .F. ) ;
#13504 = ORIENTED_EDGE ( 'NONE', *, *, #12780, .F. ) ;
#13505 = CARTESIAN_POINT ( 'NONE',  ( 0.3148213771069364175, 11.24846294176323447, -7.888490156175093304 ) ) ;
#13506 = ADVANCED_FACE ( 'NONE', ( #17564, #10395 ), #4473, .T. ) ;
#13507 = ORIENTED_EDGE ( 'NONE', *, *, #1534, .T. ) ;
#13508 = FACE_OUTER_BOUND ( 'NONE', #14460, .T. ) ;
#13509 = ORIENTED_EDGE ( 'NONE', *, *, #7813, .T. ) ;
#13510 = CARTESIAN_POINT ( 'NONE',  ( 8.438534575730034959, 0.2320579683291088824, -6.862570336891073097 ) ) ;
#13511 = CARTESIAN_POINT ( 'NONE',  ( 0.3058872367615230181, -13.72992299905060598, 0.6080468242580479021 ) ) ;
#13512 = CARTESIAN_POINT ( 'NONE',  ( 1.560000000000000053, 1.299038105676658228, -0.7500000000000009992 ) ) ;
#13513 = CARTESIAN_POINT ( 'NONE',  ( 0.3308579732647023430, -13.25341063505878481, 3.680601586799824076 ) ) ;
#13514 = CARTESIAN_POINT ( 'NONE',  ( 1.845756295923373758, 7.694561132136944259, 9.776763338604617104 ) ) ;
#13516 = CARTESIAN_POINT ( 'NONE',  ( 16.56753206892534891, 0.006760771273036174887, 0.006669401563384942146 ) ) ;
#13515 = SHAPE_REPRESENTATION ( 'High-Hardness Steel Cutting Wheel', ( #2030 ), #13001 ) ;
#13517 = FILL_AREA_STYLE_COLOUR ( '', #8423 ) ;
#13518 = CARTESIAN_POINT ( 'NONE',  ( 16.56782317627811096, -0.002708056627498708728, -0.009439921864426879458 ) ) ;
#13519 = CARTESIAN_POINT ( 'NONE',  ( 0.8740764193769091639, -3.609949042658162188, -13.83508774436024957 ) ) ;
#13520 = APPLICATION_CONTEXT ( 'automotive_design' ) ;
#13521 = DIRECTION ( 'NONE',  ( -1.000000000000000000, -0.000000000000000000, -0.000000000000000000 ) ) ;
#13522 = CARTESIAN_POINT ( 'NONE',  ( 2.697797270744668463, 12.33058466479268844, 4.970631985779629503 ) ) ;
#13523 = EDGE_CURVE ( 'NONE', #4326, #12620, #3210, .T. ) ;
#13524 = CARTESIAN_POINT ( 'NONE',  ( 22.75000000000000000, 0.000000000000000000, 0.000000000000000000 ) ) ;
#13525 = FACE_OUTER_BOUND ( 'NONE', #6195, .T. ) ;
#13526 = ORIENTED_EDGE ( 'NONE', *, *, #13769, .F. ) ;
#13527 = AXIS2_PLACEMENT_3D ( 'NONE', #7517, #3672, #3284 ) ;
#13528 = VERTEX_POINT ( 'NONE', #3111 ) ;
#13529 = ORIENTED_EDGE ( 'NONE', *, *, #17018, .F. ) ;
#13530 = ORIENTED_EDGE ( 'NONE', *, *, #16833, .T. ) ;
#13531 = EDGE_CURVE ( 'NONE', #13773, #9066, #8572, .T. ) ;
#13532 = CARTESIAN_POINT ( 'NONE',  ( 3.950837973638675393, -2.591948120961706792, -14.31366178983255466 ) ) ;
#13533 = CARTESIAN_POINT ( 'NONE',  ( 0.4385251269669950269, -13.84299131624728929, -0.7363879510386833749 ) ) ;
#13534 = CARTESIAN_POINT ( 'NONE',  ( 16.56822296793089322, 0.009385634690642057770, -0.003834730849371914118 ) ) ;
#13535 = FACE_OUTER_BOUND ( 'NONE', #5752, .T. ) ;
#13536 = CARTESIAN_POINT ( 'NONE',  ( 3.950837973638677170, 10.51028938476232355, -10.05648675950114956 ) ) ;
#13537 = ORIENTED_EDGE ( 'NONE', *, *, #8544, .T. ) ;
#13538 = DIRECTION ( 'NONE',  ( 0.000000000000000000, 0.000000000000000000, -1.000000000000000000 ) ) ;
#13539 = CARTESIAN_POINT ( 'NONE',  ( 16.57778382496167424, 0.001819584982831895037, 0.01482878558584693578 ) ) ;
#13540 = CARTESIAN_POINT ( 'NONE',  ( 0.3145734862173244495, 7.825584895511528138, 11.29227530924448430 ) ) ;
#13541 = VECTOR ( 'NONE', #7422, 1000.000000000000000 ) ;
#13542 = CARTESIAN_POINT ( 'NONE',  ( 0.000000000000000000, -1.732050807568877859, -1.752539433813135784E-17 ) ) ;
#13543 = CARTESIAN_POINT ( 'NONE',  ( 3.353306896162453477, -12.02594772223101494, 7.069984850384768649 ) ) ;
#13544 = LINE ( 'NONE', #5035, #16433 ) ;
#13545 = DIRECTION ( 'NONE',  ( 0.000000000000000000, 0.000000000000000000, 1.000000000000000000 ) ) ;
#13546 = FACE_OUTER_BOUND ( 'NONE', #10788, .T. ) ;
#13547 = ORIENTED_EDGE ( 'NONE', *, *, #18076, .T. ) ;
#13548 = VERTEX_POINT ( 'NONE', #13358 ) ;
#13549 = ADVANCED_FACE ( 'NONE', ( #6102 ), #1799, .T. ) ;
#13550 = EDGE_LOOP ( 'NONE', ( #13049, #16315 ) ) ;
#13551 = ORIENTED_EDGE ( 'NONE', *, *, #5157, .F. ) ;
#13552 = CARTESIAN_POINT ( 'NONE',  ( 1.846613052777651198, -7.585914669018095857, -9.862487290071081603 ) ) ;
#13553 = DIRECTION ( 'NONE',  ( -1.000000000000000000, 6.938893903907227392E-16, 0.000000000000000000 ) ) ;
#13554 = CIRCLE ( 'NONE', #4384, 2.499999999999995115 ) ;
#13555 = CIRCLE ( 'NONE', #5309, 7.000000000000000000 ) ;
#13556 = LINE ( 'NONE', #16441, #16640 ) ;
#13557 = CARTESIAN_POINT ( 'NONE',  ( 1.342453679581834924, 13.74702459364884533, 5.476372339890065000 ) ) ;
#13558 = PRODUCT_DEFINITION_FORMATION_WITH_SPECIFIED_SOURCE ( 'ANY', '', #16234, .NOT_KNOWN. ) ;
#13559 = CARTESIAN_POINT ( 'NONE',  ( 3.512766787570899663, 10.87507422923878586, 10.40533104696127076 ) ) ;
#13560 = ORIENTED_EDGE ( 'NONE', *, *, #15488, .T. ) ;
#13561 = CARTESIAN_POINT ( 'NONE',  ( 5.322906077793303048, 7.499999999999998224, -16.88078391064166084 ) ) ;
#13562 = CARTESIAN_POINT ( 'NONE',  ( 0.4754618798421162973, -3.583352865732575943, -13.45049478164063395 ) ) ;
#13563 = DIRECTION ( 'NONE',  ( 1.000000000000000000, -0.000000000000000000, -0.000000000000000000 ) ) ;
#13564 = CARTESIAN_POINT ( 'NONE',  ( 16.58200780006414732, -0.004047297414157817463, -0.01041078477703986926 ) ) ;
#13565 = CARTESIAN_POINT ( 'NONE',  ( -30.00000000000000355, -12.50000000000000178, -0.5000000000000000000 ) ) ;
#13566 = SURFACE_STYLE_FILL_AREA ( #7663 ) ;
#13567 = ORIENTED_EDGE ( 'NONE', *, *, #4292, .F. ) ;
#13569 = VECTOR ( 'NONE', #8522, 1000.000000000000000 ) ;
#13568 = DIRECTION ( 'NONE',  ( -1.000000000000000000, -0.000000000000000000, -0.000000000000000000 ) ) ;
#13571 = ORIENTED_EDGE ( 'NONE', *, *, #6196, .T. ) ;
#13570 = CARTESIAN_POINT ( 'NONE',  ( 1.846613052777651420, 11.72395935470504291, -4.166957398589727468 ) ) ;
#13572 = CARTESIAN_POINT ( 'NONE',  ( 2.002547531651519996, -12.57989064830760206, 0.6781519942171299054 ) ) ;
#13573 = AXIS2_PLACEMENT_3D ( 'NONE', #2229, #13609, #10746 ) ;
#13574 = EDGE_CURVE ( 'NONE', #11775, #6348, #9831, .T. ) ;
#13575 = EDGE_CURVE ( 'NONE', #10202, #11719, #6575, .T. ) ;
#13576 = ADVANCED_FACE ( 'NONE', ( #3694 ), #2084, .T. ) ;
#13577 = AXIS2_PLACEMENT_3D ( 'NONE', #8873, #1809, #87 ) ;
#13578 = CARTESIAN_POINT ( 'NONE',  ( 2.636624412714236865, 15.91454522070173638, 2.161493821596668585 ) ) ;
#13579 = ORIENTED_EDGE ( 'NONE', *, *, #12637, .F. ) ;
#13580 = CARTESIAN_POINT ( 'NONE',  ( 5.000000000000000000, 20.00000000000000000, 4.000000000000000000 ) ) ;
#13581 = CARTESIAN_POINT ( 'NONE',  ( -0.2633197948916921605, -7.500000000000000888, -14.20553286501775858 ) ) ;
#13582 = ORIENTED_EDGE ( 'NONE', *, *, #1838, .F. ) ;
#13583 = DIRECTION ( 'NONE',  ( -0.5547001962252284812, -0.8320502943378440541, 0.000000000000000000 ) ) ;
#13584 = CARTESIAN_POINT ( 'NONE',  ( 0.4385251269669942498, -10.76637725024245462, -8.732456510146192841 ) ) ;
#13585 = CIRCLE ( 'NONE', #2580, 5.000000000000000000 ) ;
#13586 = CARTESIAN_POINT ( 'NONE',  ( 0.3095370825347224519, 11.38092634279628790, 7.700448427571914500 ) ) ;
#13587 = AXIS2_PLACEMENT_3D ( 'NONE', #4016, #15666, #2564 ) ;
#13588 = CARTESIAN_POINT ( 'NONE',  ( 1.560000000000000053, -0.8660254037844384856, -1.500000000000000000 ) ) ;
#13589 = AXIS2_PLACEMENT_3D ( 'NONE', #10092, #15922, #17653 ) ;
#13590 = B_SPLINE_CURVE_WITH_KNOTS ( 'NONE', 3,
 ( #8704, #11304, #5456, #11486, #4122, #5539 ),
 .UNSPECIFIED., .F., .F.,
 ( 4, 2, 4 ),
 ( 4.206917491929696500E-17, 0.0002014099069817275648, 0.0004028198139634130625 ),
 .UNSPECIFIED. ) ;
#13591 = ORIENTED_EDGE ( 'NONE', *, *, #408, .F. ) ;
#13592 = CARTESIAN_POINT ( 'NONE',  ( 1.846138399168762101, 12.43476674860266584, 0.4167076046095977149 ) ) ;
#13593 =( BOUNDED_SURFACE ( )  B_SPLINE_SURFACE ( 3, 1, ( 
 ( #6290, #13736 ),
 ( #10589, #9521 ),
 ( #13539, #458 ),
 ( #4757, #10779 ) ),
 .UNSPECIFIED., .F., .F., .T. ) 
 B_SPLINE_SURFACE_WITH_KNOTS ( ( 4, 4 ),
 ( 2, 2 ),
 ( 0.000000000000000000, 1.000000000000000000 ),
 ( 0.000000000000000000, 1.000000000000000000 ),
 .UNSPECIFIED. ) 
 GEOMETRIC_REPRESENTATION_ITEM ( )  RATIONAL_B_SPLINE_SURFACE ( (
 ( 1.000000000000000000, 1.000000000000000000),
 ( 0.7792777138730160313, 0.9689936506012927220),
 ( 0.7792777138730160313, 0.9689936506012927220),
 ( 1.000000000000000000, 1.000000000000000000) ) ) 
 REPRESENTATION_ITEM ( '' )  SURFACE ( )  );
#13594 = CARTESIAN_POINT ( 'NONE',  ( 15.00000000000000711, -39.99999999999999289, 3.000000000000000000 ) ) ;
#13596 = EDGE_LOOP ( 'NONE', ( #7325, #3660, #13874, #8364 ) ) ;
#13595 = CARTESIAN_POINT ( 'NONE',  ( 1.959212340397942675, 10.53510106265292023, -6.829000156128068433 ) ) ;
#13597 = CARTESIAN_POINT ( 'NONE',  ( 2.747332970342022840, -11.66639548242798696, -11.45495994260730654 ) ) ;
#13598 = B_SPLINE_CURVE_WITH_KNOTS ( 'NONE', 3,
 ( #713, #5193, #5009, #12277, #5104, #15045 ),
 .UNSPECIFIED., .F., .F.,
 ( 4, 2, 4 ),
 ( 4.240893905418535831E-17, 0.0002014099069817285406, 0.0004028198139634146346 ),
 .UNSPECIFIED. ) ;
#13599 = VECTOR ( 'NONE', #5620, 1000.000000000000114 ) ;
#13600 = ORIENTED_EDGE ( 'NONE', *, *, #6801, .T. ) ;
#13601 = CARTESIAN_POINT ( 'NONE',  ( 2.002547531651519996, 11.75462648437101976, 4.532360870844369671 ) ) ;
#13602 = CARTESIAN_POINT ( 'NONE',  ( 3.353306896162453921, -13.88482890973695660, -1.348936822032970495 ) ) ;
#13603 = AXIS2_PLACEMENT_3D ( 'NONE', #10198, #72, #8861 ) ;
#13604 = ORIENTED_EDGE ( 'NONE', *, *, #12565, .T. ) ;
#13605 = EDGE_LOOP ( 'NONE', ( #3018, #7974, #9513, #13070 ) ) ;
#13606 = DIRECTION ( 'NONE',  ( 1.000000000000000000, -0.000000000000000000, -0.000000000000000000 ) ) ;
#13607 = EDGE_CURVE ( 'NONE', #13957, #16055, #715, .T. ) ;
#13608 = ORIENTED_EDGE ( 'NONE', *, *, #3211, .F. ) ;
#13609 = DIRECTION ( 'NONE',  ( 0.000000000000000000, -1.000000000000000000, 0.000000000000000000 ) ) ;
#13610 = ADVANCED_FACE ( 'NONE', ( #8106 ), #16727, .F. ) ;
#13611 = ORIENTED_EDGE ( 'NONE', *, *, #15246, .F. ) ;
#13612 = DIRECTION ( 'NONE',  ( 0.000000000000000000, 0.000000000000000000, -1.000000000000000000 ) ) ;
#13613 = DIRECTION ( 'NONE',  ( -1.000000000000000000, -0.000000000000000000, -0.000000000000000000 ) ) ;
#13614 = CARTESIAN_POINT ( 'NONE',  ( 16.56679352167444819, 0.001518074900130650254, -0.009170718284672547266 ) ) ;
#13615 = LINE ( 'NONE', #10949, #7235 ) ;
#13616 = EDGE_CURVE ( 'NONE', #13920, #5818, #5426, .T. ) ;
#13617 = DIRECTION ( 'NONE',  ( 0.9034263296138843602, 0.000000000000000000, 0.4287433579198459133 ) ) ;
#13618 = CARTESIAN_POINT ( 'NONE',  ( 2.747332970342022840, -2.409922051470793747, 16.17136872824897864 ) ) ;
#13619 = AXIS2_PLACEMENT_3D ( 'NONE', #16365, #16265, #6330 ) ;
#13620 = CARTESIAN_POINT ( 'NONE',  ( 3.950837973638668288, 14.41405733518061716, 1.958075594453843493 ) ) ;
#13621 = CARTESIAN_POINT ( 'NONE',  ( 1.845756295923353996, 3.386818134580228179, -11.97166802574122890 ) ) ;
#13622 = ORIENTED_EDGE ( 'NONE', *, *, #14005, .F. ) ;
#13623 = CARTESIAN_POINT ( 'NONE',  ( 0.3095370825347233956, -8.444334731363927204, -10.84046130709067590 ) ) ;
#13624 = CARTESIAN_POINT ( 'NONE',  ( 2.636624412714242194, 14.46769361191244485, 6.973567714906650394 ) ) ;
#13625 = PRODUCT_RELATED_PRODUCT_CATEGORY ( 'part', '', ( #16234 ) ) ;
#13626 = CARTESIAN_POINT ( 'NONE',  ( 1.846955891736118849, -11.91257079808165820, -3.593597880662470878 ) ) ;
#13627 = CARTESIAN_POINT ( 'NONE',  ( 2.123976203522053741, -13.47898556379307244, -7.899625852120357727 ) ) ;
#13628 = EDGE_CURVE ( 'NONE', #2337, #347, #13050, .T. ) ;
#13629 = EDGE_LOOP ( 'NONE', ( #17701, #13126, #4237, #4476 ) ) ;
#13630 = VERTEX_POINT ( 'NONE', #18135 ) ;
#13631 = EDGE_CURVE ( 'NONE', #7533, #3542, #13544, .T. ) ;
#13632 = ORIENTED_EDGE ( 'NONE', *, *, #10826, .T. ) ;
#13633 = EDGE_CURVE ( 'NONE', #17649, #18897, #10884, .T. ) ;
#13634 = AXIS2_PLACEMENT_3D ( 'NONE', #5482, #17149, #8458 ) ;
#13635 = EDGE_LOOP ( 'NONE', ( #2724, #17768, #4577, #18341 ) ) ;
#13636 = MECHANICAL_DESIGN_GEOMETRIC_PRESENTATION_REPRESENTATION (  '', ( #12418 ), #2624 ) ;
#13637 = CARTESIAN_POINT ( 'NONE',  ( 0.3151926232592501265, 4.318679262939624230, 13.04305446098357635 ) ) ;
#13638 = CARTESIAN_POINT ( 'NONE',  ( 1.562796894703937678, 0.000000000000000000, 0.000000000000000000 ) ) ;
#13639 = CARTESIAN_POINT ( 'NONE',  ( 1.847034903785823579, -12.44051878787772836, -0.2299360331935480506 ) ) ;
#13640 = CARTESIAN_POINT ( 'NONE',  ( 16.56782317627811096, 0.009228812961909594811, 0.003357783021327272015 ) ) ;
#13641 = CARTESIAN_POINT ( 'NONE',  ( 1.959283090834855745, -12.53713130127478337, 0.6676170829051779609 ) ) ;
#13642 = PRODUCT_DEFINITION_CONTEXT ( 'detailed design', #13520, 'design' ) ;
#13643 = CIRCLE ( 'NONE', #1417, 2.499999999999995115 ) ;
#13644 = CARTESIAN_POINT ( 'NONE',  ( 3.074695600507708182, 10.75417554975745205, 11.23985886659407463 ) ) ;
#13645 = CARTESIAN_POINT ( 'NONE',  ( 1.847372867223024295, -11.86627781945711568, 3.744745203533932365 ) ) ;
#13646 = AXIS2_PLACEMENT_3D ( 'NONE', #18496, #15914, #14102 ) ;
#13647 = EDGE_CURVE ( 'NONE', #15590, #17568, #277, .T. ) ;
#13648 = MECHANICAL_DESIGN_GEOMETRIC_PRESENTATION_REPRESENTATION (  '', ( #4169 ), #10915 ) ;
#13649 = CARTESIAN_POINT ( 'NONE',  ( 2.747332970342022840, -2.705255688517959722, 16.12459247543625551 ) ) ;
#13650 = CARTESIAN_POINT ( 'NONE',  ( 1.959212340397945562, -11.71715421693495074, -4.509090217468642692 ) ) ;
#13651 = DIRECTION ( 'NONE',  ( -1.000000000000000000, -0.000000000000000000, -0.000000000000000000 ) ) ;
#13652 = AXIS2_PLACEMENT_3D ( 'NONE', #4305, #2842, #10130 ) ;
#13653 = CARTESIAN_POINT ( 'NONE',  ( 16.58200780006414732, -0.008650561019685852962, -0.007066318000005976374 ) ) ;
#13654 = VECTOR ( 'NONE', #9316, 1000.000000000000000 ) ;
#13655 = ORIENTED_EDGE ( 'NONE', *, *, #14692, .T. ) ;
#13656 = PRODUCT_DEFINITION_SHAPE ( 'NONE', 'NONE',  #18909 ) ;
#13657 = ORIENTED_EDGE ( 'NONE', *, *, #17078, .T. ) ;
#13658 = ORIENTED_EDGE ( 'NONE', *, *, #7688, .F. ) ;
#13659 = VECTOR ( 'NONE', #9775, 1000.000000000000000 ) ;
#13660 = ORIENTED_EDGE ( 'NONE', *, *, #14666, .F. ) ;
#13661 = CARTESIAN_POINT ( 'NONE',  ( 0.3137051932979792457, -13.73004976592201842, -0.4596302728641207813 ) ) ;
#13662 = AXIS2_PLACEMENT_3D ( 'NONE', #9202, #16658, #18003 ) ;
#13663 = CARTESIAN_POINT ( 'NONE',  ( 2.123976203522053741, 13.47898556379313284, 7.899625852120258251 ) ) ;
#13664 = CARTESIAN_POINT ( 'NONE',  ( 1.846613052777651198, -7.585914669018095857, -9.862487290071081603 ) ) ;
#13665 = CARTESIAN_POINT ( 'NONE',  ( 3.074695600507264537, -13.70113613813205689, 7.366518011945889732 ) ) ;
#13666 = CARTESIAN_POINT ( 'NONE',  ( 0.8740779401508622648, 0.8420120399581700887, 14.27348745891572968 ) ) ;
#13667 = VERTEX_POINT ( 'NONE', #16704 ) ;
#13668 = CARTESIAN_POINT ( 'NONE',  ( 0.3132635586635982294, 3.740017578711948953, -13.21855946425832684 ) ) ;
#13669 = CARTESIAN_POINT ( 'NONE',  ( 0.3095370825347234511, -3.806662003783320980, -13.20347358821918426 ) ) ;
#13670 = CARTESIAN_POINT ( 'NONE',  ( -1.715145640899952140, 6.797472175340259604, -12.00000001230413460 ) ) ;
#13671 = CARTESIAN_POINT ( 'NONE',  ( 1.847372867223027848, -10.12831093686727080, 7.228345833872717563 ) ) ;
#13672 = CARTESIAN_POINT ( 'NONE',  ( 16.56782317627811096, -0.007739510688078479403, 0.006045301465876602373 ) ) ;
#13673 = EDGE_CURVE ( 'NONE', #6835, #12288, #12350, .T. ) ;
#13674 = CARTESIAN_POINT ( 'NONE',  ( 2.697797270744668019, -0.9169917281808188658, 13.26309265156976913 ) ) ;
#13675 = CARTESIAN_POINT ( 'NONE',  ( 0.3142014840576518031, 0.3830336514510798707, -13.73311050063163563 ) ) ;
#13676 = EDGE_LOOP ( 'NONE', ( #59, #16575, #7498, #10067 ) ) ;
#13677 = CARTESIAN_POINT ( 'NONE',  ( 2.750000000000000000, 0.000000000000000000, 0.000000000000000000 ) ) ;
#13679 = ORIENTED_EDGE ( 'NONE', *, *, #5746, .F. ) ;
#13678 = DIRECTION ( 'NONE',  ( -1.000000000000000000, -0.000000000000000000, -0.000000000000000000 ) ) ;
#13680 = CARTESIAN_POINT ( 'NONE',  ( -194.9999999999999716, 9.999999999999973355, 6.000000000000000000 ) ) ;
#13681 = VECTOR ( 'NONE', #15619, 1000.000000000000000 ) ;
#13682 = ORIENTED_EDGE ( 'NONE', *, *, #17218, .T. ) ;
#13683 = DIRECTION ( 'NONE',  ( 0.000000000000000000, 0.000000000000000000, 1.000000000000000000 ) ) ;
#13684 = CARTESIAN_POINT ( 'NONE',  ( -0.09864563712516453975, -7.002566078024231366, -11.99999999788115446 ) ) ;
#13685 = ORIENTED_EDGE ( 'NONE', *, *, #17591, .T. ) ;
#13686 = CARTESIAN_POINT ( 'NONE',  ( 16.57210152137263393, -0.01361613799508851197, -0.005118120558001528972 ) ) ;
#13687 = CARTESIAN_POINT ( 'NONE',  ( 16.56822296793089322, -0.007741272030791128758, -0.006547366384935482571 ) ) ;
#13688 = CARTESIAN_POINT ( 'NONE',  ( 2.636624412715137922, -15.91454522070252153, 2.161493821597598508 ) ) ;
#13689 = CARTESIAN_POINT ( 'NONE',  ( 2.636624412714236865, 15.91454522070173638, 2.161493821596668585 ) ) ;
#13690 = ADVANCED_FACE ( 'NONE', ( #11063 ), #6554, .F. ) ;
#13691 = EDGE_CURVE ( 'NONE', #13818, #5518, #9991, .T. ) ;
#13692 = EDGE_CURVE ( 'NONE', #13860, #1293, #1769, .T. ) ;
#13693 = EDGE_LOOP ( 'NONE', ( #7086, #14917, #9123, #2825 ) ) ;
#13694 =( LENGTH_UNIT ( ) NAMED_UNIT ( * ) SI_UNIT ( .MILLI., .METRE. ) );
#13695 = FACE_OUTER_BOUND ( 'NONE', #309, .T. ) ;
#13696 = PLANE ( 'NONE',  #11647 ) ;
#13698 = EDGE_LOOP ( 'NONE', ( #16596, #5637 ) ) ;
#13697 = CARTESIAN_POINT ( 'NONE',  ( 0.000000000000000000, 0.000000000000000000, 11.00000000000000000 ) ) ;
#13699 = CARTESIAN_POINT ( 'NONE',  ( 0.3720661004400037664, 10.73619472937702213, 8.694226082900630814 ) ) ;
#13700 = ORIENTED_EDGE ( 'NONE', *, *, #14047, .F. ) ;
#13701 = CARTESIAN_POINT ( 'NONE',  ( 1.560000000000000053, 1.732050807568878747, 7.017607234860990640E-28 ) ) ;
#13702 = CARTESIAN_POINT ( 'NONE',  ( 1.977436885025426250, 7.806953934146316776, 13.27782258181756880 ) ) ;
#13703 = ADVANCED_FACE ( 'NONE', ( #6479 ), #3606, .T. ) ;
#13704 = VERTEX_POINT ( 'NONE', #15442 ) ;
#13705 = ORIENTED_EDGE ( 'NONE', *, *, #15715, .T. ) ;
#13706 = CARTESIAN_POINT ( 'NONE',  ( 0.3137051932979775248, 10.83767969834815581, -8.442169467526731808 ) ) ;
#13707 = ORIENTED_EDGE ( 'NONE', *, *, #10780, .T. ) ;
#13708 = CARTESIAN_POINT ( 'NONE',  ( 0.3095370825347233956, 11.38092634279628967, 7.700448427571912724 ) ) ;
#13709 = ORIENTED_EDGE ( 'NONE', *, *, #1998, .F. ) ;
#13710 = FILL_AREA_STYLE_COLOUR ( '', #7952 ) ;
#13711 = DIRECTION ( 'NONE',  ( -0.000000000000000000, 1.000000000000000000, -0.000000000000000000 ) ) ;
#13712 = DIRECTION ( 'NONE',  ( -0.9034263296138843602, 0.000000000000000000, -0.4287433579198459133 ) ) ;
#13713 = CARTESIAN_POINT ( 'NONE',  ( 2.636624412716902288, 7.605649742760546950, -14.14563173255513995 ) ) ;
#13714 = CARTESIAN_POINT ( 'NONE',  ( 8.438534575730034959, -6.598402093327893958, 1.899950616255162483 ) ) ;
#13715 =( BOUNDED_SURFACE ( )  B_SPLINE_SURFACE ( 3, 1, ( 
 ( #436, #9129 ),
 ( #6265, #12197 ),
 ( #2237, #18022 ),
 ( #8080, #16497 ) ),
 .UNSPECIFIED., .F., .F., .T. ) 
 B_SPLINE_SURFACE_WITH_KNOTS ( ( 4, 4 ),
 ( 2, 2 ),
 ( 0.000000000000000000, 1.000000000000000000 ),
 ( 0.000000000000000000, 1.000000000000000000 ),
 .UNSPECIFIED. ) 
 GEOMETRIC_REPRESENTATION_ITEM ( )  RATIONAL_B_SPLINE_SURFACE ( (
 ( 1.000000000000000000, 1.000000000000000000),
 ( 0.7792777138730158093, 0.9689936506012928330),
 ( 0.7792777138730158093, 0.9689936506012928330),
 ( 1.000000000000000000, 1.000000000000000000) ) ) 
 REPRESENTATION_ITEM ( '' )  SURFACE ( )  );
#13716 = CARTESIAN_POINT ( 'NONE',  ( 16.56872352241294521, -0.004907101719995745834, -0.009207754980064182873 ) ) ;
#13717 = DIRECTION ( 'NONE',  ( 1.000000000000000000, 0.000000000000000000, -0.000000000000000000 ) ) ;
#13718 = EDGE_CURVE ( 'NONE', #18215, #15699, #14381, .T. ) ;
#13719 = CARTESIAN_POINT ( 'NONE',  ( 3.664313757352970047, -9.645155442698829518, 10.50730552161229880 ) ) ;
#13720 = DIRECTION ( 'NONE',  ( -0.7635533937278214944, -0.3966532189476559833, -0.5095610256143900951 ) ) ;
#13721 = CARTESIAN_POINT ( 'NONE',  ( 1.977228804422632713, -13.27756617201330336, -7.806978995470745808 ) ) ;
#13722 = CARTESIAN_POINT ( 'NONE',  ( 0.3132635586635976188, -7.641727604903970850, 11.41586812343486912 ) ) ;
#13723 = AXIS2_PLACEMENT_3D ( 'NONE', #13353, #7248, #5991 ) ;
#13724 = ORIENTED_EDGE ( 'NONE', *, *, #14910, .T. ) ;
#13725 = STYLED_ITEM ( 'NONE', ( #15785 ), #3708 ) ;
#13726 = EDGE_CURVE ( 'NONE', #16462, #13012, #2965, .T. ) ;
#13727 = ORIENTED_EDGE ( 'NONE', *, *, #664, .F. ) ;
#13728 = ORIENTED_EDGE ( 'NONE', *, *, #8829, .T. ) ;
#13729 = ORIENTED_EDGE ( 'NONE', *, *, #9135, .T. ) ;
#13730 = EDGE_LOOP ( 'NONE', ( #5398, #5212, #3493, #994 ) ) ;
#13731 = COLOUR_RGB ( '', 0.31764706, 0.68627451, 0.89019608) ;
#13732 = CARTESIAN_POINT ( 'NONE',  ( 0.3142014840576536905, 10.88517824918543297, 8.382000553815492694 ) ) ;
#13733 = CARTESIAN_POINT ( 'NONE',  ( 1.149044392847440088, -7.500000000000001776, -14.62466132081333292 ) ) ;
#13734 = CARTESIAN_POINT ( 'NONE',  ( 1.861706995891669880, 9.751699138048550708, -7.751853334747211832 ) ) ;
#13735 = VERTEX_POINT ( 'NONE', #14099 ) ;
#13736 = CARTESIAN_POINT ( 'NONE',  ( 0.4754618798421167414, 13.89949764182682657, 0.7484603771384882309 ) ) ;
#13737 = FACE_OUTER_BOUND ( 'NONE', #5894, .T. ) ;
#13738 = DIRECTION ( 'NONE',  ( 1.000000000000000000, 0.000000000000000000, 0.000000000000000000 ) ) ;
#13739 = CARTESIAN_POINT ( 'NONE',  ( 1.254255976358044311, -7.789651112956927470, -12.44256109021856105 ) ) ;
#13740 = DIRECTION ( 'NONE',  ( -1.000000000000000000, -0.000000000000000000, -0.000000000000000000 ) ) ;
#13741 = ORIENTED_EDGE ( 'NONE', *, *, #12412, .F. ) ;
#13742 = EDGE_CURVE ( 'NONE', #8095, #8500, #5308, .T. ) ;
#13743 = ORIENTED_EDGE ( 'NONE', *, *, #9796, .F. ) ;
#13744 = ORIENTED_EDGE ( 'NONE', *, *, #5472, .T. ) ;
#13745 =( BOUNDED_SURFACE ( )  B_SPLINE_SURFACE ( 3, 1, ( 
 ( #1344, #1446 ),
 ( #7283, #13102 ),
 ( #17493, #4400 ),
 ( #10234, #16060 ) ),
 .UNSPECIFIED., .F., .F., .T. ) 
 B_SPLINE_SURFACE_WITH_KNOTS ( ( 4, 4 ),
 ( 2, 2 ),
 ( 0.000000000000000000, 1.000000000000000000 ),
 ( 0.000000000000000000, 1.000000000000000000 ),
 .UNSPECIFIED. ) 
 GEOMETRIC_REPRESENTATION_ITEM ( )  RATIONAL_B_SPLINE_SURFACE ( (
 ( 1.000000000000000000, 1.000000000000000000),
 ( 0.9933953342250438912, 0.8357391271907739227),
 ( 0.9933953342250438912, 0.8357391271907739227),
 ( 1.000000000000000000, 1.000000000000000000) ) ) 
 REPRESENTATION_ITEM ( '' )  SURFACE ( )  );
#13746 = ORIENTED_EDGE ( 'NONE', *, *, #10451, .T. ) ;
#13747 = CARTESIAN_POINT ( 'NONE',  ( 2.179449471770337432, -4.500000000000000000, -3.000000000000000000 ) ) ;
#13748 = EDGE_CURVE ( 'NONE', #15007, #8344, #1289, .T. ) ;
#13749 = CARTESIAN_POINT ( 'NONE',  ( 3.950837973638676281, -1.958075594453890789, 14.41405733518059940 ) ) ;
#13750 = CARTESIAN_POINT ( 'NONE',  ( 1.847372867223024961, -7.228345833872678483, -10.12831093686730100 ) ) ;
#13751 = CARTESIAN_POINT ( 'NONE',  ( 3.074695600507349358, 10.75417554975707368, -11.23985886659415279 ) ) ;
#13752 = DIRECTION ( 'NONE',  ( -1.000000000000000000, 0.000000000000000000, 0.000000000000000000 ) ) ;
#13753 = ORIENTED_EDGE ( 'NONE', *, *, #16735, .F. ) ;
#13754 = CARTESIAN_POINT ( 'NONE',  ( 1.342453679581834924, -11.38190519890846453, -9.456403821038923851 ) ) ;
#13755 = CARTESIAN_POINT ( 'NONE',  ( 2.123976203522053297, -15.26039569100261950, 3.347755036805843076 ) ) ;
#13756 = CARTESIAN_POINT ( 'NONE',  ( -0.1927609796802092212, 7.499999999999999112, -14.19253746125318116 ) ) ;
#13757 = CARTESIAN_POINT ( 'NONE',  ( 16.56753206892534891, -0.009369540855502119653, -0.001549402974393242162 ) ) ;
#13758 = CARTESIAN_POINT ( 'NONE',  ( -66.35602477868049220, -10.00000000000000888, 5.999999999999999112 ) ) ;
#13759 = DIRECTION ( 'NONE',  ( -1.000000000000000000, 0.000000000000000000, 0.000000000000000000 ) ) ;
#13760 = B_SPLINE_CURVE_WITH_KNOTS ( 'NONE', 3,
 ( #7557, #1425, #184, #12981, #11559, #6013, #284, #6113, #1610, #16041, #17775, #7266, #4678 ),
 .UNSPECIFIED., .F., .F.,
 ( 4, 3, 3, 3, 4 ),
 ( 2.168404344971008868E-18, 0.0002299804304191468746, 0.0004599608082120234371, 0.0006467586077648000654, 0.0008336169836825981817 ),
 .UNSPECIFIED. ) ;
#13761 = B_SPLINE_CURVE_WITH_KNOTS ( 'NONE', 3,
 ( #18170, #2121, #18434, #12432, #15480, #9742 ),
 .UNSPECIFIED., .F., .F.,
 ( 4, 2, 4 ),
 ( 3.361796080452501619E-17, 0.0001825746017570592115, 0.0003651492035140848128 ),
 .UNSPECIFIED. ) ;
#13762 = VERTEX_POINT ( 'NONE', #14298 ) ;
#13763 = B_SPLINE_CURVE_WITH_KNOTS ( 'NONE', 3,
 ( #7470, #7859, #7576, #1927, #6416, #3341 ),
 .UNSPECIFIED., .F., .F.,
 ( 4, 2, 4 ),
 ( 0.000000000000000000, 0.001656992708822557434, 0.003313985417645114867 ),
 .UNSPECIFIED. ) ;
#13765 = ORIENTED_EDGE ( 'NONE', *, *, #14050, .T. ) ;
#13764 = CARTESIAN_POINT ( 'NONE',  ( 0.4754618798421171855, -10.80499583390519192, 8.775436892861074867 ) ) ;
#13766 = CARTESIAN_POINT ( 'NONE',  ( 0.4862570985993235340, -12.97920246947883172, 5.003653737315437944 ) ) ;
#13767 = EDGE_CURVE ( 'NONE', #6138, #4723, #2354, .T. ) ;
#13768 = AXIS2_PLACEMENT_3D ( 'NONE', #13354, #8772, #13061 ) ;
#13769 = EDGE_CURVE ( 'NONE', #10942, #9252, #4166, .T. ) ;
#13770 = ORIENTED_EDGE ( 'NONE', *, *, #2678, .T. ) ;
#13771 = DIRECTION ( 'NONE',  ( 1.000000000000000000, 0.000000000000000000, 0.000000000000000000 ) ) ;
#13772 = CARTESIAN_POINT ( 'NONE',  ( 0.6634400264851448847, -7.500000000000235367, -13.04619536630284493 ) ) ;
#13773 = VERTEX_POINT ( 'NONE', #8196 ) ;
#13774 = DIRECTION ( 'NONE',  ( 0.000000000000000000, 0.000000000000000000, -1.000000000000000000 ) ) ;
#13775 = CARTESIAN_POINT ( 'NONE',  ( 2.002547531651519996, 6.845637710436341727, -10.57595306287284842 ) ) ;
#13776 = APPLICATION_CONTEXT ( 'automotive_design' ) ;
#13777 = CARTESIAN_POINT ( 'NONE',  ( 1.861628059977341154, -11.66985327793196170, -4.358833901513171405 ) ) ;
#13778 = PLANE ( 'NONE',  #1684 ) ;
#13779 = SHAPE_REPRESENTATION_RELATIONSHIP ( 'NONE' , 'NONE' ,  #4478, #18307 ) ;
#13780 = CARTESIAN_POINT ( 'NONE',  ( 16.57778382496167424, -0.006312874906843772387, 0.01354073047775764503 ) ) ;
#13781 = CARTESIAN_POINT ( 'NONE',  ( -112.7602355015299338, -81.60345299795268659, -92.39524324337544670 ) ) ;
#13783 = ORIENTED_EDGE ( 'NONE', *, *, #4670, .T. ) ;
#13782 = CARTESIAN_POINT ( 'NONE',  ( -2.500000000000000000, 3.061616997868383141E-16, -3.000000000000000000 ) ) ;
#13784 = CARTESIAN_POINT ( 'NONE',  ( 4.755015822784811164, -4.336808689942017736E-16, 0.000000000000000000 ) ) ;
#13785 = ORIENTED_EDGE ( 'NONE', *, *, #10925, .T. ) ;
#13786 = DIRECTION ( 'NONE',  ( -0.000000000000000000, 0.5000000000000004441, 0.8660254037844383745 ) ) ;
#13787 = CARTESIAN_POINT ( 'NONE',  ( -4.000000000000000000, 20.00000000000000000, 7.000000000000000000 ) ) ;
#13788 = VERTEX_POINT ( 'NONE', #9615 ) ;
#13789 = EDGE_CURVE ( 'NONE', #11533, #1561, #13258, .T. ) ;
#13790 = ORIENTED_EDGE ( 'NONE', *, *, #14203, .T. ) ;
#13791 = LINE ( 'NONE', #11220, #3548 ) ;
#13792 = DIRECTION ( 'NONE',  ( 0.000000000000000000, 0.000000000000000000, 1.000000000000000000 ) ) ;
#13793 = ORIENTED_EDGE ( 'NONE', *, *, #388, .F. ) ;
#13794 = LINE ( 'NONE', #18436, #10240 ) ;
#13795 = FACE_OUTER_BOUND ( 'NONE', #14366, .T. ) ;
#13796 = AXIS2_PLACEMENT_3D ( 'NONE', #13747, #659, #3615 ) ;
#13797 = CARTESIAN_POINT ( 'NONE',  ( -199.9999999999999716, 4.999999999999974243, 3.000000000000000000 ) ) ;
#13798 = CARTESIAN_POINT ( 'NONE',  ( 15.00000000000000711, -18.99999999999999645, 8.000000000000000000 ) ) ;
#13799 = FACE_OUTER_BOUND ( 'NONE', #636, .T. ) ;
#13800 = APPLICATION_PROTOCOL_DEFINITION ( 'draft international standard', 'automotive_design', 1998, #7049 ) ;
#13801 = CARTESIAN_POINT ( 'NONE',  ( 1.959212340397942675, 10.53510106265292023, -6.829000156128068433 ) ) ;
#13802 = CARTESIAN_POINT ( 'NONE',  ( 3.950837973638677170, 12.81214529934985080, -6.888253895133152227 ) ) ;
#13803 = CARTESIAN_POINT ( 'NONE',  ( 1.847247051441592181, 7.448813758297314180, -9.967131402978116839 ) ) ;
#13804 = CARTESIAN_POINT ( 'NONE',  ( 3.950837973638668288, 14.41405733518061538, -1.958075594453841273 ) ) ;
#13805 = CARTESIAN_POINT ( 'NONE',  ( 1.846138399168762101, 12.43476674860266584, 0.4167076046095977149 ) ) ;
#13806 = CONICAL_SURFACE ( 'NONE', #16258, 14.54644660717763927, 0.8559913436420816257 ) ;
#13807 = CARTESIAN_POINT ( 'NONE',  ( 16.57778382496167424, -0.01018821665058785610, 0.01092721432668990016 ) ) ;
#13808 = ORIENTED_EDGE ( 'NONE', *, *, #7200, .T. ) ;
#13809 = ADVANCED_FACE ( 'NONE', ( #16976 ), #4510, .T. ) ;
#13810 = ADVANCED_FACE ( 'NONE', ( #15816 ), #18123, .F. ) ;
#13811 = EDGE_CURVE ( 'NONE', #12951, #1583, #15532, .T. ) ;
#13812 = EDGE_LOOP ( 'NONE', ( #6252, #4030, #13027, #2601 ) ) ;
#13813 = ORIENTED_EDGE ( 'NONE', *, *, #2695, .T. ) ;
#13814 = ORIENTED_EDGE ( 'NONE', *, *, #13334, .T. ) ;
#13815 = CARTESIAN_POINT ( 'NONE',  ( 0.3132635586635977853, 12.89236642382228126, -4.743936529203109487 ) ) ;
#13816 =( BOUNDED_SURFACE ( )  B_SPLINE_SURFACE ( 3, 1, ( 
 ( #6757, #14009 ),
 ( #9705, #8281 ),
 ( #14294, #14096 ),
 ( #15439, #1094 ) ),
 .UNSPECIFIED., .F., .F., .T. ) 
 B_SPLINE_SURFACE_WITH_KNOTS ( ( 4, 4 ),
 ( 2, 2 ),
 ( 0.000000000000000000, 1.000000000000000000 ),
 ( 0.000000000000000000, 1.000000000000000000 ),
 .UNSPECIFIED. ) 
 GEOMETRIC_REPRESENTATION_ITEM ( )  RATIONAL_B_SPLINE_SURFACE ( (
 ( 1.000000000000000000, 1.000000000000000000),
 ( 0.7792777138730160313, 0.9689936506012927220),
 ( 0.7792777138730160313, 0.9689936506012927220),
 ( 1.000000000000000000, 1.000000000000000000) ) ) 
 REPRESENTATION_ITEM ( '' )  SURFACE ( )  );
#13817 = LINE ( 'NONE', #733, #12355 ) ;
#13818 = VERTEX_POINT ( 'NONE', #18675 ) ;
#13819 = CARTESIAN_POINT ( 'NONE',  ( 2.002547531651519996, -12.57989064830759141, -0.6781519942173057647 ) ) ;
#13820 = FACE_OUTER_BOUND ( 'NONE', #15159, .T. ) ;
#13821 = CARTESIAN_POINT ( 'NONE',  ( 0.3939822652208145870, 10.75310269629521365, 8.678192463540208124 ) ) ;
#13822 = LINE ( 'NONE', #7927, #1295 ) ;
#13823 = CARTESIAN_POINT ( 'NONE',  ( 1.861628059977343819, -7.751680370225458638, 9.751736252960339968 ) ) ;
#13824 = CARTESIAN_POINT ( 'NONE',  ( 0.3132642857406526260, 8.495623922778223758, -10.79548167658025193 ) ) ;
#13825 = CARTESIAN_POINT ( 'NONE',  ( 16.56872352241294521, 0.004564908236399969378, -0.009382111268607383134 ) ) ;
#13826 = CIRCLE ( 'NONE', #7118, 5.000000000000000000 ) ;
#13827 = VERTEX_POINT ( 'NONE', #9789 ) ;
#13828 = ORIENTED_EDGE ( 'NONE', *, *, #1779, .F. ) ;
#13829 = ORIENTED_EDGE ( 'NONE', *, *, #14023, .T. ) ;
#13830 = ORIENTED_EDGE ( 'NONE', *, *, #4688, .T. ) ;
#13831 = DIRECTION ( 'NONE',  ( -1.000000000000000000, -0.000000000000000000, -0.000000000000000000 ) ) ;
#13832 = ADVANCED_FACE ( 'NONE', ( #11430 ), #15643, .F. ) ;
#13833 = CARTESIAN_POINT ( 'NONE',  ( 2.747332970342022840, 14.49942876448592521, 7.555624153089699924 ) ) ;
#13834 = EDGE_CURVE ( 'NONE', #11551, #9965, #943, .T. ) ;
#13835 = AXIS2_PLACEMENT_3D ( 'NONE', #9209, #16488, #1859 ) ;
#13836 = CARTESIAN_POINT ( 'NONE',  ( 1.560000000000000053, -0.8660254037844384856, -1.500000000000000000 ) ) ;
#13837 = CARTESIAN_POINT ( 'NONE',  ( 16.56872352241294521, 0.001442253899401220278, -0.01033355228142500415 ) ) ;
#13838 = VERTEX_POINT ( 'NONE', #8842 ) ;
#13839 = CARTESIAN_POINT ( 'NONE',  ( 8.522092701127531811, 1.786985377232127137, -6.722964936702079619 ) ) ;
#13840 = B_SPLINE_CURVE_WITH_KNOTS ( 'NONE', 3,
 ( #17361, #5884, #8482, #1404, #14311, #11727 ),
 .UNSPECIFIED., .F., .F.,
 ( 4, 2, 4 ),
 ( 2.239080928920849783E-18, 0.0002017457492448096685, 0.0004034914984896170601 ),
 .UNSPECIFIED. ) ;
#13841 = VECTOR ( 'NONE', #11208, 1000.000000000000114 ) ;
#13842 = CARTESIAN_POINT ( 'NONE',  ( 0.000000000000000000, -2.375000000000000444, -4.362804221962445569E-16 ) ) ;
#13843 = CARTESIAN_POINT ( 'NONE',  ( -0.8060261380169082557, 7.500000000000031086, -13.05296413415600298 ) ) ;
#13844 = CARTESIAN_POINT ( 'NONE',  ( 1.918921323896325415, -7.860085869556248994, 9.738309537478970768 ) ) ;
#13845 = CYLINDRICAL_SURFACE ( 'NONE', #16662, 5.000000000000000888 ) ;
#13846 = DIRECTION ( 'NONE',  ( 0.000000000000000000, 0.000000000000000000, 1.000000000000000000 ) ) ;
#13847 = DIRECTION ( 'NONE',  ( -0.000000000000000000, -0.000000000000000000, 1.000000000000000000 ) ) ;
#13848 = DIRECTION ( 'NONE',  ( -1.000000000000000000, -0.000000000000000000, -0.000000000000000000 ) ) ;
#13849 = ORIENTED_EDGE ( 'NONE', *, *, #3155, .T. ) ;
#13851 = ORIENTED_EDGE ( 'NONE', *, *, #7813, .F. ) ;
#13850 = DIRECTION ( 'NONE',  ( 0.000000000000000000, 0.000000000000000000, 1.000000000000000000 ) ) ;
#13852 = CARTESIAN_POINT ( 'NONE',  ( 0.4754618798421167414, -12.98792082933641012, -5.007009103465385635 ) ) ;
#13853 = CIRCLE ( 'NONE', #3156, 5.000000000000000888 ) ;
#13854 = PRESENTATION_LAYER_ASSIGNMENT (  '', '', ( #14462 ) ) ;
#13855 = ADVANCED_FACE ( 'NONE', ( #4548 ), #13329, .T. ) ;
#13856 = VERTEX_POINT ( 'NONE', #4352 ) ;
#13857 = DIRECTION ( 'NONE',  ( 0.000000000000000000, 0.000000000000000000, 1.000000000000000000 ) ) ;
#13858 = EDGE_CURVE ( 'NONE', #3595, #8004, #15524, .T. ) ;
#13859 = CARTESIAN_POINT ( 'NONE',  ( -0.03525595549294711917, -7.500000000000000888, -14.17755750872192522 ) ) ;
#13860 = VERTEX_POINT ( 'NONE', #4641 ) ;
#13861 = CARTESIAN_POINT ( 'NONE',  ( 2.697797270744666243, 8.537712152181008207, -10.19107313879048249 ) ) ;
#13862 = CARTESIAN_POINT ( 'NONE',  ( 0.4862570985993235340, -13.44146924561383827, 3.580942890621619412 ) ) ;
#13863 = CARTESIAN_POINT ( 'NONE',  ( 1.254009781011620417, -14.64464726212587919, 1.011465182608038305 ) ) ;
#13864 = FACE_OUTER_BOUND ( 'NONE', #13241, .T. ) ;
#13865 = AXIS2_PLACEMENT_3D ( 'NONE', #1646, #12076, #10645 ) ;
#13866 = EDGE_CURVE ( 'NONE', #4817, #14724, #7803, .T. ) ;
#13867 =( NAMED_UNIT ( * ) PLANE_ANGLE_UNIT ( ) SI_UNIT ( $, .RADIAN. ) );
#13868 = CARTESIAN_POINT ( 'NONE',  ( 8.438534575730034959, -2.341351102130233119, -6.454982381540311565 ) ) ;
#13869 = CARTESIAN_POINT ( 'NONE',  ( 3.950837973638668288, 0.000000000000000000, 0.000000000000000000 ) ) ;
#13871 = ORIENTED_EDGE ( 'NONE', *, *, #7117, .F. ) ;
#13870 = DIRECTION ( 'NONE',  ( -0.7561779333270775005, 0.03481510524964793324, 0.6534392409364820908 ) ) ;
#13872 = CARTESIAN_POINT ( 'NONE',  ( 2.636624412716061627, -7.605649742761058540, -14.14563173255469408 ) ) ;
#13873 = EDGE_CURVE ( 'NONE', #18002, #7476, #10937, .T. ) ;
#13874 = ORIENTED_EDGE ( 'NONE', *, *, #16986, .T. ) ;
#13875 = CARTESIAN_POINT ( 'NONE',  ( 1.560000000000000053, -1.732050807568877859, -1.752539433813135784E-17 ) ) ;
#13876 = CARTESIAN_POINT ( 'NONE',  ( 16.56782317627811096, 0.006045301465876368185, -0.007739510688079533247 ) ) ;
#13877 = ORIENTED_EDGE ( 'NONE', *, *, #15551, .F. ) ;
#13878 = AXIS2_PLACEMENT_3D ( 'NONE', #8481, #14310, #12865 ) ;
#13879 = VERTEX_POINT ( 'NONE', #7324 ) ;
#13880 = DIRECTION ( 'NONE',  ( 0.000000000000000000, 0.000000000000000000, -1.000000000000000000 ) ) ;
#13881 = APPLICATION_CONTEXT ( 'automotive_design' ) ;
#13882 = CARTESIAN_POINT ( 'NONE',  ( 16.56782317627811096, -0.003357783021327886107, -0.009228812961908644183 ) ) ;
#13883 = EDGE_LOOP ( 'NONE', ( #10577, #18590, #13095, #12993 ) ) ;
#13884 = CIRCLE ( 'NONE', #9905, 2.499999999999995115 ) ;
#13885 = CARTESIAN_POINT ( 'NONE',  ( 0.4862570985993235340, 3.580942890621860109, -13.44146924561377254 ) ) ;
#13886 = FACE_OUTER_BOUND ( 'NONE', #8789, .T. ) ;
#13887 = CARTESIAN_POINT ( 'NONE',  ( 2.320520222536938348, -1.795797593768547085, 15.64520721754664123 ) ) ;
#13888 = CARTESIAN_POINT ( 'NONE',  ( 3.686287386450715076E-15, -27.00000000000000000, 25.01316734529526187 ) ) ;
#13889 =( NAMED_UNIT ( * ) SI_UNIT ( $, .STERADIAN. ) SOLID_ANGLE_UNIT ( ) );
#13890 = CONTEXT_DEPENDENT_SHAPE_REPRESENTATION ( #9964, #18080 ) ;
#13891 =( LENGTH_UNIT ( ) NAMED_UNIT ( * ) SI_UNIT ( .MILLI., .METRE. ) );
#13892 = CARTESIAN_POINT ( 'NONE',  ( 2.500000000000000000, 0.000000000000000000, -13.00000000000000533 ) ) ;
#13893 = EDGE_CURVE ( 'NONE', #6155, #8319, #1387, .T. ) ;
#13894 = CARTESIAN_POINT ( 'NONE',  ( 8.438534575730034959, -5.688336279099072357, 3.845978796786017284 ) ) ;
#13895 = AXIS2_PLACEMENT_3D ( 'NONE', #15302, #18270, #2214 ) ;
#13896 = CIRCLE ( 'NONE', #18475, 4.999999999999997335 ) ;
#13897 = CARTESIAN_POINT ( 'NONE',  ( 2.002547531651519996, -7.942910686618240845, 9.778737580845669797 ) ) ;
#13898 = CARTESIAN_POINT ( 'NONE',  ( 0.8740764193767950330, -14.27348595579787371, -0.8420116711623154560 ) ) ;
#13899 = CARTESIAN_POINT ( 'NONE',  ( 0.4384471787762820871, -13.39294437382615399, -3.577367180593688634 ) ) ;
#13900 = FACE_OUTER_BOUND ( 'NONE', #17076, .T. ) ;
#13901 = VERTEX_POINT ( 'NONE', #16202 ) ;
#13902 = VERTEX_POINT ( 'NONE', #7228 ) ;
#13903 = ORIENTED_EDGE ( 'NONE', *, *, #11831, .F. ) ;
#13904 = ORIENTED_EDGE ( 'NONE', *, *, #16501, .T. ) ;
#13905 = ORIENTED_EDGE ( 'NONE', *, *, #8435, .F. ) ;
#13906 = AXIS2_PLACEMENT_3D ( 'NONE', #6454, #18109, #12095 ) ;
#13907 = STYLED_ITEM ( 'NONE', ( #12372 ), #2583 ) ;
#13908 = CARTESIAN_POINT ( 'NONE',  ( 0.3137051932979792457, 11.37800749014131263, 7.698472063774513430 ) ) ;
#13909 = CARTESIAN_POINT ( 'NONE',  ( 5.342326914280424610, -7.500000000000001776, -16.88455910646441538 ) ) ;
#13910 = DIRECTION ( 'NONE',  ( -0.7561779333270775005, -0.2350349629540143537, -0.6106991889125079620 ) ) ;
#13911 = CARTESIAN_POINT ( 'NONE',  ( -20.00000000000000000, -2.500000000000000444, -17.00000000000000000 ) ) ;
#13912 = EDGE_CURVE ( 'NONE', #2507, #4747, #3084, .T. ) ;
#13913 = FACE_OUTER_BOUND ( 'NONE', #1942, .T. ) ;
#13914 = EDGE_CURVE ( 'NONE', #14481, #14993, #8457, .T. ) ;
#13915 = DIRECTION ( 'NONE',  ( -0.000000000000000000, -0.000000000000000000, -1.000000000000000000 ) ) ;
#13916 = EDGE_CURVE ( 'NONE', #6081, #17016, #47, .T. ) ;
#13917 = DIRECTION ( 'NONE',  ( -0.000000000000000000, -0.000000000000000000, 1.000000000000000000 ) ) ;
#13918 = CARTESIAN_POINT ( 'NONE',  ( 1.861706995891668770, 7.751853334747318414, 9.751699138048461890 ) ) ;
#13919 = LINE ( 'NONE', #7931, #16700 ) ;
#13920 = VERTEX_POINT ( 'NONE', #6075 ) ;
#13921 = AXIS2_PLACEMENT_3D ( 'NONE', #2365, #3798, #5235 ) ;
#13922 = VERTEX_POINT ( 'NONE', #8930 ) ;
#13923 = ORIENTED_EDGE ( 'NONE', *, *, #2463, .F. ) ;
#13924 = VERTEX_POINT ( 'NONE', #13426 ) ;
#13925 = EDGE_CURVE ( 'NONE', #6600, #9356, #9036, .T. ) ;
#13926 = CARTESIAN_POINT ( 'NONE',  ( 1.846138399168762101, -7.646096044339819819, -9.815003036200495856 ) ) ;
#13927 =( BOUNDED_SURFACE ( )  B_SPLINE_SURFACE ( 3, 1, ( 
 ( #14371, #1276 ),
 ( #17335, #4252 ),
 ( #11797, #4629 ),
 ( #14946, #3173 ) ),
 .UNSPECIFIED., .F., .F., .T. ) 
 B_SPLINE_SURFACE_WITH_KNOTS ( ( 4, 4 ),
 ( 2, 2 ),
 ( 0.000000000000000000, 1.000000000000000000 ),
 ( 0.000000000000000000, 1.000000000000000000 ),
 .UNSPECIFIED. ) 
 GEOMETRIC_REPRESENTATION_ITEM ( )  RATIONAL_B_SPLINE_SURFACE ( (
 ( 1.000000000000000000, 1.000000000000000000),
 ( 0.9933953342250436691, 0.8357391271907733676),
 ( 0.9933953342250436691, 0.8357391271907733676),
 ( 1.000000000000000000, 1.000000000000000000) ) ) 
 REPRESENTATION_ITEM ( '' )  SURFACE ( )  );
#13928 = DIRECTION ( 'NONE',  ( -1.000000000000000000, -0.000000000000000000, -0.000000000000000000 ) ) ;
#13929 = CARTESIAN_POINT ( 'NONE',  ( 3.950837973638668288, 0.000000000000000000, 0.000000000000000000 ) ) ;
#13930 = FACE_OUTER_BOUND ( 'NONE', #3098, .T. ) ;
#13931 = DIRECTION ( 'NONE',  ( -1.000000000000000000, 0.000000000000000000, 0.000000000000000000 ) ) ;
#13932 = EDGE_LOOP ( 'NONE', ( #14942, #2358, #925, #1261 ) ) ;
#13933 = CARTESIAN_POINT ( 'NONE',  ( 2.747332970342022840, -11.66639548242798696, -11.45495994260730654 ) ) ;
#13934 = CIRCLE ( 'NONE', #13335, 7.000000000000000000 ) ;
#13935 = CARTESIAN_POINT ( 'NONE',  ( 1.254255976357310010, 7.789651112956863521, 12.44256109021772438 ) ) ;
#13936 = CARTESIAN_POINT ( 'NONE',  ( -2.166051897649948543, 7.500000000000000000, -13.14980647003224767 ) ) ;
#13937 = DIRECTION ( 'NONE',  ( -0.000000000000000000, 0.5000000000000004441, 0.8660254037844383745 ) ) ;
#13938 = MECHANICAL_DESIGN_GEOMETRIC_PRESENTATION_REPRESENTATION (  '', ( #3857 ), #217 ) ;
#13939 = CIRCLE ( 'NONE', #2939, 4.000000000000000000 ) ;
#13940 = DIRECTION ( 'NONE',  ( -1.000000000000000000, 0.000000000000000000, 0.000000000000000000 ) ) ;
#13941 = CARTESIAN_POINT ( 'NONE',  ( 3.512766787570714477, -14.81029789862161117, -2.682019731918549255 ) ) ;
#13942 = CARTESIAN_POINT ( 'NONE',  ( 0.3142014840576536905, 10.88517824918543297, 8.382000553815492694 ) ) ;
#13943 = ORIENTED_EDGE ( 'NONE', *, *, #16449, .T. ) ;
#13944 = EDGE_CURVE ( 'NONE', #7599, #16462, #6955, .T. ) ;
#13945 = EDGE_CURVE ( 'NONE', #1518, #11387, #1578, .T. ) ;
#13946 = AXIS2_PLACEMENT_3D ( 'NONE', #9753, #17395, #968 ) ;
#13948 = ORIENTED_EDGE ( 'NONE', *, *, #15267, .F. ) ;
#13947 = CARTESIAN_POINT ( 'NONE',  ( 2.747332970342022840, -11.66639548242815572, 11.45495994260713957 ) ) ;
#13949 = CARTESIAN_POINT ( 'NONE',  ( -194.9999999999999716, 4.999999999999973355, 3.000000000000002665 ) ) ;
#13950 = AXIS2_PLACEMENT_3D ( 'NONE', #904, #18385, #2504 ) ;
#13951 = AXIS2_PLACEMENT_3D ( 'NONE', #6963, #5503, #11351 ) ;
#13952 = EDGE_CURVE ( 'NONE', #15103, #11694, #14758, .T. ) ;
#13953 = ORIENTED_EDGE ( 'NONE', *, *, #9268, .T. ) ;
#13954 = CARTESIAN_POINT ( 'NONE',  ( 2.002547531651519996, 11.75462648437101976, 4.532360870844369671 ) ) ;
#13955 = CARTESIAN_POINT ( 'NONE',  ( -26.50000000000001066, -12.50000000000000178, 6.000000000000000000 ) ) ;
#13956 = B_SPLINE_CURVE_WITH_KNOTS ( 'NONE', 3,
 ( #13624, #3676, #3769, #10669, #18116, #5016 ),
 .UNSPECIFIED., .F., .F.,
 ( 4, 2, 4 ),
 ( 0.000000000000000000, 0.001656992708822033113, 0.003313985417644066227 ),
 .UNSPECIFIED. ) ;
#13957 = VERTEX_POINT ( 'NONE', #341 ) ;
#13958 = CARTESIAN_POINT ( 'NONE',  ( 1.846955891736119293, -7.098901504650428684, 10.21904526726843798 ) ) ;
#13959 = CARTESIAN_POINT ( 'NONE',  ( 0.3307726912345197445, 13.74203354050372106, -0.5948952607473121379 ) ) ;
#13960 = CARTESIAN_POINT ( 'NONE',  ( 0.3137051932979757485, -8.442169467526770887, -10.83767969834812561 ) ) ;
#13961 = FACE_OUTER_BOUND ( 'NONE', #16979, .T. ) ;
#13962 = CARTESIAN_POINT ( 'NONE',  ( 3.074695600507237891, -15.41438262616227739, 2.093687500611889352 ) ) ;
#13963 =( NAMED_UNIT ( * ) PLANE_ANGLE_UNIT ( ) SI_UNIT ( $, .RADIAN. ) );
#13964 = CARTESIAN_POINT ( 'NONE',  ( 2.636624412714237309, 15.80357026013209953, 2.862162146984226663 ) ) ;
#13965 = EDGE_CURVE ( 'NONE', #16993, #17332, #17602, .T. ) ;
#13966 = EDGE_CURVE ( 'NONE', #12106, #5602, #17635, .T. ) ;
#13967 = CARTESIAN_POINT ( 'NONE',  ( -30.00000000000000355, -12.50000000000000178, 3.000000000000000000 ) ) ;
#13969 = ORIENTED_EDGE ( 'NONE', *, *, #14784, .T. ) ;
#13968 = CARTESIAN_POINT ( 'NONE',  ( 3.950837973638675393, -13.10350451991845055, 6.316429227969417859 ) ) ;
#13970 = CARTESIAN_POINT ( 'NONE',  ( 1.136128737974912818E-14, -9.013167318348349610, 27.61316734529538053 ) ) ;
#13971 = VECTOR ( 'NONE', #5867, 1000.000000000000000 ) ;
#13972 = CARTESIAN_POINT ( 'NONE',  ( 16.56822296793089322, -0.008619100080559813359, -0.005339139727952636229 ) ) ;
#13973 = CARTESIAN_POINT ( 'NONE',  ( 16.57210152137263393, -0.01402404281922924566, 0.003862718596009228310 ) ) ;
#13974 = CARTESIAN_POINT ( 'NONE',  ( 0.3148208552358936485, -4.463611911212133521, -12.99355031785210102 ) ) ;
#13975 = EDGE_CURVE ( 'NONE', #9622, #14131, #11243, .T. ) ;
#13976 = ORIENTED_EDGE ( 'NONE', *, *, #7260, .F. ) ;
#13977 = ORIENTED_EDGE ( 'NONE', *, *, #2888, .F. ) ;
#13978 = CARTESIAN_POINT ( 'NONE',  ( 1.959283090834838870, -9.750336807931205385, 7.909254450748972154 ) ) ;
#13979 = CARTESIAN_POINT ( 'NONE',  ( 2.636624412715137922, -6.973567714907947135, 14.46769361191283920 ) ) ;
#13980 = ORIENTED_EDGE ( 'NONE', *, *, #5054, .T. ) ;
#13981 = CARTESIAN_POINT ( 'NONE',  ( -194.9999999999999716, 9.999999999999973355, 3.000000000000000000 ) ) ;
#13982 = EDGE_CURVE ( 'NONE', #14041, #4291, #15060, .T. ) ;
#13983 = CARTESIAN_POINT ( 'NONE',  ( 1.861706995891668104, 6.878962591851903063, -10.38589138506418408 ) ) ;
#13984 = PRESENTATION_STYLE_ASSIGNMENT (( #12631 ) ) ;
#13985 = LINE ( 'NONE', #712, #9324 ) ;
#13986 = DIRECTION ( 'NONE',  ( 0.000000000000000000, 0.000000000000000000, 1.000000000000000000 ) ) ;
#13987 = CIRCLE ( 'NONE', #12461, 2.749999999999996891 ) ;
#13988 = APPLICATION_PROTOCOL_DEFINITION ( 'draft international standard', 'automotive_design', 1998, #8629 ) ;
#13989 =( NAMED_UNIT ( * ) SI_UNIT ( $, .STERADIAN. ) SOLID_ANGLE_UNIT ( ) );
#13990 = CARTESIAN_POINT ( 'NONE',  ( 2.749999999999998224, 0.000000000000000000, 7.000000000000000000 ) ) ;
#13991 = CARTESIAN_POINT ( 'NONE',  ( 0.3150692679895942816, -13.11337225490255776, 4.099798979280796729 ) ) ;
#13992 = B_SPLINE_CURVE_WITH_KNOTS ( 'NONE', 3,
 ( #249, #18874, #12003, #13333, #8845, #10572, #14572, #5972, #17448, #5869, #17541, #14667, #4354 ),
 .UNSPECIFIED., .F., .F.,
 ( 4, 3, 3, 3, 4 ),
 ( 3.198396408832238080E-18, 0.0002299780670421061189, 0.0004599561239687905540, 0.0006896788984287883888, 0.0009194956271626399547 ),
 .UNSPECIFIED. ) ;
#13993 = DIRECTION ( 'NONE',  ( -1.000000000000000000, -0.000000000000000000, -0.000000000000000000 ) ) ;
#13994 = DIRECTION ( 'NONE',  ( -0.000000000000000000, -0.5000000000000003331, -0.8660254037844384856 ) ) ;
#13995 = CARTESIAN_POINT ( 'NONE',  ( 1.959283090834856189, 12.53713130127477804, -0.6676170829052656686 ) ) ;
#13996 =( NAMED_UNIT ( * ) PLANE_ANGLE_UNIT ( ) SI_UNIT ( $, .RADIAN. ) );
#13997 = VERTEX_POINT ( 'NONE', #8081 ) ;
#13998 = EDGE_CURVE ( 'NONE', #698, #16167, #18204, .T. ) ;
#13999 = ORIENTED_EDGE ( 'NONE', *, *, #13093, .F. ) ;
#14000 = B_SPLINE_CURVE_WITH_KNOTS ( 'NONE', 3,
 ( #16371, #4803, #10534, #16562, #3450, #1841, #9284, #15116, #2034, #9000, #18084, #16645, #3253 ),
 .UNSPECIFIED., .F., .F.,
 ( 4, 3, 3, 3, 4 ),
 ( 3.198396408832238080E-18, 0.0002299780670421061189, 0.0004599561239687905540, 0.0006896788984287883888, 0.0009194956271626399547 ),
 .UNSPECIFIED. ) ;
#14001 = EDGE_LOOP ( 'NONE', ( #14031, #1856, #9418, #11069 ) ) ;
#14002 = ORIENTED_EDGE ( 'NONE', *, *, #13523, .T. ) ;
#14003 = CIRCLE ( 'NONE', #14744, 5.000000000000000000 ) ;
#14004 = VERTEX_POINT ( 'NONE', #17933 ) ;
#14005 = EDGE_CURVE ( 'NONE', #16346, #16292, #10734, .T. ) ;
#14006 = DIRECTION ( 'NONE',  ( 0.000000000000000000, 0.000000000000000000, -1.000000000000000000 ) ) ;
#14007 = CARTESIAN_POINT ( 'NONE',  ( -3.605312816022526956, -7.500000000000002665, -16.26975837274199677 ) ) ;
#14008 = CARTESIAN_POINT ( 'NONE',  ( 8.438534575730034959, -6.862570336891073985, -0.2320579683290849293 ) ) ;
#14009 = CARTESIAN_POINT ( 'NONE',  ( 0.4754618798421167414, 7.564402563418470393, 11.68486377711969126 ) ) ;
#14010 = CARTESIAN_POINT ( 'NONE',  ( 20.00000000000000000, 7.499999999999999112, -12.00000000000000000 ) ) ;
#14011 = CARTESIAN_POINT ( 'NONE',  ( 0.4384471787762852513, 7.540925784514715957, -11.63197976518319798 ) ) ;
#14012 = DIRECTION ( 'NONE',  ( 1.000000000000000000, 0.000000000000000000, 0.000000000000000000 ) ) ;
#14013 = VECTOR ( 'NONE', #4300, 1000.000000000000114 ) ;
#14014 = CARTESIAN_POINT ( 'NONE',  ( 16.56753206892534891, 0.006760771273036169683, 0.006669401563384943880 ) ) ;
#14015 = CARTESIAN_POINT ( 'NONE',  ( 16.56872352241294521, 0.001442253899401802278, 0.01033355228142402403 ) ) ;
#14016 = ORIENTED_EDGE ( 'NONE', *, *, #16986, .F. ) ;
#14017 = ORIENTED_EDGE ( 'NONE', *, *, #2062, .F. ) ;
#14018 = VECTOR ( 'NONE', #2729, 1000.000000000000000 ) ;
#14019 = VERTEX_POINT ( 'NONE', #16591 ) ;
#14020 =( REPRESENTATION_RELATIONSHIP ('NONE','NONE', #5200, #6437 ) REPRESENTATION_RELATIONSHIP_WITH_TRANSFORMATION ( #7012 )SHAPE_REPRESENTATION_RELATIONSHIP( ) );
#14021 = EDGE_LOOP ( 'NONE', ( #17988, #14185, #6957, #13743, #18391 ) ) ;
#14022 = EDGE_CURVE ( 'NONE', #8344, #13257, #9397, .T. ) ;
#14023 = EDGE_CURVE ( 'NONE', #3394, #11870, #8232, .T. ) ;
#14024 = EDGE_CURVE ( 'NONE', #5848, #5701, #9701, .T. ) ;
#14025 = DIRECTION ( 'NONE',  ( -0.7635533937278216055, 0.6453904417649387604, -0.02138673900302117195 ) ) ;
#14026 = AXIS2_PLACEMENT_3D ( 'NONE', #12793, #4383, #2742 ) ;
#14027 = CARTESIAN_POINT ( 'NONE',  ( -2.749999999999997335, 3.367778697655217560E-16, 7.000000000000000000 ) ) ;
#14028 = CARTESIAN_POINT ( 'NONE',  ( 2.123976203522053297, -13.47898556379318435, 7.899625852120161440 ) ) ;
#14029 = DIRECTION ( 'NONE',  ( 0.000000000000000000, 0.000000000000000000, 1.000000000000000000 ) ) ;
#14030 = CARTESIAN_POINT ( 'NONE',  ( 2.747332970342022840, -2.705255688517733681, -16.12459247543629104 ) ) ;
#14031 = ORIENTED_EDGE ( 'NONE', *, *, #4337, .T. ) ;
#14032 = CARTESIAN_POINT ( 'NONE',  ( 16.56753206892534891, 0.001421777558676785977, 0.009389754735541558373 ) ) ;
#14033 = LINE ( 'NONE', #937, #12035 ) ;
#14034 = CARTESIAN_POINT ( 'NONE',  ( -5.343731732829805736, 7.499999999999999112, -16.88485148858611140 ) ) ;
#14035 = CARTESIAN_POINT ( 'NONE',  ( 2.636624412714134280, 2.862162146984768896, 15.80357026013147426 ) ) ;
#14036 = CYLINDRICAL_SURFACE ( 'NONE', #5062, 2.499999999999992006 ) ;
#14037 = CARTESIAN_POINT ( 'NONE',  ( 0.000000000000000000, -2.375000000000000444, -4.362804221962445569E-16 ) ) ;
#14038 = B_SPLINE_CURVE_WITH_KNOTS ( 'NONE', 3,
 ( #5862, #2986, #3079, #14753, #1664, #4923 ),
 .UNSPECIFIED., .F., .F.,
 ( 4, 2, 4 ),
 ( 8.673617379884034509E-19, 0.0001828790815886950508, 0.0003657581631773892342 ),
 .UNSPECIFIED. ) ;
#14039 = CARTESIAN_POINT ( 'NONE',  ( 12.00000000000000711, -18.99999999999999645, 8.000000000000000000 ) ) ;
#14040 = CARTESIAN_POINT ( 'NONE',  ( 0.3142011359265333148, 11.33549115679423736, 7.762194356530812023 ) ) ;
#14041 = VERTEX_POINT ( 'NONE', #16406 ) ;
#14043 = ORIENTED_EDGE ( 'NONE', *, *, #7573, .T. ) ;
#14042 = CARTESIAN_POINT ( 'NONE',  ( -27.32408120756002035, 20.00000000000000000, 3.000000000000000000 ) ) ;
#14044 = DIRECTION ( 'NONE',  ( -1.000000000000000000, -1.776356839400250465E-15, 0.000000000000000000 ) ) ;
#14045 = B_SPLINE_CURVE_WITH_KNOTS ( 'NONE', 3,
 ( #8192, #8280, #1003, #6840, #18491, #14191 ),
 .UNSPECIFIED., .F., .F.,
 ( 4, 2, 4 ),
 ( 4.336808689942017736E-19, 0.001500839035891552006, 0.003001678071783103578 ),
 .UNSPECIFIED. ) ;
#14046 = FACE_OUTER_BOUND ( 'NONE', #7040, .T. ) ;
#14047 = EDGE_CURVE ( 'NONE', #14167, #18612, #12549, .T. ) ;
#14048 = EDGE_CURVE ( 'NONE', #4379, #14416, #1873, .T. ) ;
#14049 = ORIENTED_EDGE ( 'NONE', *, *, #17474, .F. ) ;
#14050 = EDGE_CURVE ( 'NONE', #16214, #15892, #10979, .T. ) ;
#14051 = CARTESIAN_POINT ( 'NONE',  ( 16.56822296793089322, -0.002414375228568911048, -0.009847136207495301580 ) ) ;
#14052 = CARTESIAN_POINT ( 'NONE',  ( 2.500000000000000000, 0.000000000000000000, -13.00000000000000533 ) ) ;
#14053 = EDGE_CURVE ( 'NONE', #12529, #16119, #1833, .T. ) ;
#14054 = ORIENTED_EDGE ( 'NONE', *, *, #12187, .F. ) ;
#14055 = FACE_OUTER_BOUND ( 'NONE', #9619, .T. ) ;
#14056 = CARTESIAN_POINT ( 'NONE',  ( 8.522092701127531811, -1.786985377232080285, 6.722964936702092054 ) ) ;
#14057 = DIRECTION ( 'NONE',  ( 0.000000000000000000, 0.000000000000000000, 1.000000000000000000 ) ) ;
#14058 = DIRECTION ( 'NONE',  ( 0.000000000000000000, 0.000000000000000000, 1.000000000000000000 ) ) ;
#14059 = DIRECTION ( 'NONE',  ( 0.000000000000000000, -0.000000000000000000, -1.000000000000000000 ) ) ;
#14060 = SURFACE_STYLE_USAGE ( .BOTH. , #15396 ) ;
#14061 = CARTESIAN_POINT ( 'NONE',  ( 3.512766787570759774, -13.55823433651952925, 6.535475144496928124 ) ) ;
#14062 = CARTESIAN_POINT ( 'NONE',  ( 16.57778382496167424, -0.01354073047775889056, 0.006312874906844006574 ) ) ;
#14064 = ORIENTED_EDGE ( 'NONE', *, *, #12164, .T. ) ;
#14063 = LINE ( 'NONE', #11299, #2629 ) ;
#14065 = CARTESIAN_POINT ( 'NONE',  ( 16.56753206892534891, 0.004253784598196760393, 0.008490833999798020129 ) ) ;
#14066 = ORIENTED_EDGE ( 'NONE', *, *, #1455, .F. ) ;
#14067 = CARTESIAN_POINT ( 'NONE',  ( 1.846138399168762101, 11.95493567637855392, -3.446241763652874379 ) ) ;
#14068 = CARTESIAN_POINT ( 'NONE',  ( 2.002547531651519996, 4.532360870844494016, -11.75462648437097180 ) ) ;
#14069 = ORIENTED_EDGE ( 'NONE', *, *, #5290, .T. ) ;
#14070 = ORIENTED_EDGE ( 'NONE', *, *, #6862, .F. ) ;
#14071 = CARTESIAN_POINT ( 'NONE',  ( 8.522092701127531811, -6.722964936702111594, 1.786985377232005900 ) ) ;
#14072 = CARTESIAN_POINT ( 'NONE',  ( 0.3142014840576518031, 0.3830336514510798707, -13.73311050063163563 ) ) ;
#14073 = VERTEX_POINT ( 'NONE', #718 ) ;
#14074 = CARTESIAN_POINT ( 'NONE',  ( 0.000000000000000000, 0.000000000000000000, 7.000000000000000000 ) ) ;
#14075 = CARTESIAN_POINT ( 'NONE',  ( 1.977228804422745068, 3.321884655131805975, -15.04020501276218091 ) ) ;
#14076 = AXIS2_PLACEMENT_3D ( 'NONE', #5151, #16815, #9547 ) ;
#14077 = EDGE_CURVE ( 'NONE', #10867, #18304, #1460, .T. ) ;
#14078 = CARTESIAN_POINT ( 'NONE',  ( 0.3095370825347234511, -11.38092634279634119, 7.700448427571834564 ) ) ;
#14079 = DIRECTION ( 'NONE',  ( -1.000000000000000000, 0.000000000000000000, 0.000000000000000000 ) ) ;
#14080 = CARTESIAN_POINT ( 'NONE',  ( 1.918918678667045574, 12.08296592096908384, 3.258447776119875350 ) ) ;
#14081 = ITEM_DEFINED_TRANSFORMATION ( 'NONE', 'NONE', #5675,  #2030 ) ;
#14082 = CARTESIAN_POINT ( 'NONE',  ( 1.846138399168762101, 7.646096044340033870, -9.815003036200328879 ) ) ;
#14083 = PLANE ( 'NONE',  #569 ) ;
#14084 = CARTESIAN_POINT ( 'NONE',  ( 1.847247051441591958, -3.685275815977108405, -11.88474976472816103 ) ) ;
#14085 = CARTESIAN_POINT ( 'NONE',  ( 0.3170788640506441158, 4.392045232375811459, 13.02120094575829867 ) ) ;
#14086 = EDGE_CURVE ( 'NONE', #7817, #14561, #7565, .T. ) ;
#14087 = DIRECTION ( 'NONE',  ( -1.000000000000000000, -0.000000000000000000, -0.000000000000000000 ) ) ;
#14088 = ORIENTED_EDGE ( 'NONE', *, *, #14048, .T. ) ;
#14089 = ORIENTED_EDGE ( 'NONE', *, *, #12222, .F. ) ;
#14090 = ORIENTED_EDGE ( 'NONE', *, *, #6909, .T. ) ;
#14091 = CIRCLE ( 'NONE', #681, 5.000000000000000000 ) ;
#14092 = ORIENTED_EDGE ( 'NONE', *, *, #5974, .F. ) ;
#14093 = CARTESIAN_POINT ( 'NONE',  ( 1.847168016377982003, -0.1868244120188694568, -12.44137401948661292 ) ) ;
#14094 = CARTESIAN_POINT ( 'NONE',  ( 1.846138399168762101, -9.815003036200353748, -7.646096044340000120 ) ) ;
#14095 = CARTESIAN_POINT ( 'NONE',  ( 0.3095370825347234511, -0.4597470195091165057, 13.73357284481724605 ) ) ;
#14096 = CARTESIAN_POINT ( 'NONE',  ( 2.123976203522053297, 7.899625852120206737, 13.47898556379315771 ) ) ;
#14097 = DIRECTION ( 'NONE',  ( 0.000000000000000000, 0.000000000000000000, -1.000000000000000000 ) ) ;
#14098 = CARTESIAN_POINT ( 'NONE',  ( 0.3170788640506441158, 13.74111462631963576, -0.1533108587036642600 ) ) ;
#14099 = CARTESIAN_POINT ( 'NONE',  ( 0.000000000000000000, 1.732050807568878747, 7.017607234860990640E-28 ) ) ;
#14100 = CIRCLE ( 'NONE', #11665, 5.000000000000000888 ) ;
#14101 = CARTESIAN_POINT ( 'NONE',  ( 16.56872352241294521, 0.007512283835805451566, 0.007240717549634016065 ) ) ;
#14102 = DIRECTION ( 'NONE',  ( 0.000000000000000000, 0.000000000000000000, 1.000000000000000000 ) ) ;
#14103 = ADVANCED_FACE ( 'NONE', ( #2418 ), #14083, .F. ) ;
#14104 = ORIENTED_EDGE ( 'NONE', *, *, #4630, .T. ) ;
#14105 = ORIENTED_EDGE ( 'NONE', *, *, #5123, .T. ) ;
#14106 = EDGE_CURVE ( 'NONE', #14416, #11694, #11837, .T. ) ;
#14107 = EDGE_LOOP ( 'NONE', ( #18103, #14206, #6355, #125 ) ) ;
#14108 = ORIENTED_EDGE ( 'NONE', *, *, #14767, .T. ) ;
#14109 = CARTESIAN_POINT ( 'NONE',  ( 15.00000000000000711, -19.99999999999999645, 8.000000000000000000 ) ) ;
#14110 = CARTESIAN_POINT ( 'NONE',  ( 0.4754618798421162973, 7.564402563418467729, 11.68486377711969304 ) ) ;
#14111 = DIRECTION ( 'NONE',  ( -1.000000000000000000, -0.000000000000000000, -0.000000000000000000 ) ) ;
#14112 = CARTESIAN_POINT ( 'NONE',  ( 16.57210152137263393, 0.009075239946108201033, -0.01136813053532078656 ) ) ;
#14113 = ORIENTED_EDGE ( 'NONE', *, *, #18693, .T. ) ;
#14114 = CARTESIAN_POINT ( 'NONE',  ( 0.3095370825347234511, 8.444334731364163460, -10.84046130709049294 ) ) ;
#14115 = CARTESIAN_POINT ( 'NONE',  ( 1.847372867223022963, -11.80112642014552371, -3.945260592619169948 ) ) ;
#14116 = CARTESIAN_POINT ( 'NONE',  ( 6.538348415311014072, 7.499999999999999112, -17.00000000000000000 ) ) ;
#14117 = CARTESIAN_POINT ( 'NONE',  ( 0.3308579732646998450, 13.74211098745269766, 0.5950689966504839612 ) ) ;
#14118 = VECTOR ( 'NONE', #3383, 1000.000000000000000 ) ;
#14119 = CARTESIAN_POINT ( 'NONE',  ( 1.846138399168762101, 11.95493567637855392, -3.446241763652874379 ) ) ;
#14120 = CARTESIAN_POINT ( 'NONE',  ( 1.846138399168762101, -10.30487220521565028, -6.971848976711123136 ) ) ;
#14121 = CARTESIAN_POINT ( 'NONE',  ( 0.3132642857406527370, 4.743831191224565202, -12.89240536501341161 ) ) ;
#14122 = EDGE_CURVE ( 'NONE', #11616, #7718, #18473, .T. ) ;
#14123 = DIRECTION ( 'NONE',  ( 0.000000000000000000, 1.000000000000000000, 0.000000000000000000 ) ) ;
#14124 = EDGE_CURVE ( 'NONE', #12130, #18846, #3906, .T. ) ;
#14125 = ORIENTED_EDGE ( 'NONE', *, *, #4769, .F. ) ;
#14127 = ORIENTED_EDGE ( 'NONE', *, *, #11831, .T. ) ;
#14126 = CARTESIAN_POINT ( 'NONE',  ( 0.000000000000000000, 0.000000000000000000, 8.000000000000000000 ) ) ;
#14128 = FACE_OUTER_BOUND ( 'NONE', #15904, .T. ) ;
#14129 = DIRECTION ( 'NONE',  ( 0.000000000000000000, 0.000000000000000000, 1.000000000000000000 ) ) ;
#14130 = VECTOR ( 'NONE', #3234, 1000.000000000000000 ) ;
#14131 = VERTEX_POINT ( 'NONE', #6651 ) ;
#14132 = CARTESIAN_POINT ( 'NONE',  ( 1.846524061778019199, -3.506196582971023545, -11.93805390544204670 ) ) ;
#14133 = B_SPLINE_CURVE_WITH_KNOTS ( 'NONE', 3,
 ( #1176, #813, #2687, #15515 ),
 .UNSPECIFIED., .F., .F.,
 ( 4, 4 ),
 ( 0.000000000000000000, 0.002004993803842355579 ),
 .UNSPECIFIED. ) ;
#14134 = DIRECTION ( 'NONE',  ( -0.000000000000000000, -0.000000000000000000, -1.000000000000000000 ) ) ;
#14135 = CARTESIAN_POINT ( 'NONE',  ( 0.3720661004400040439, 13.34435358167253227, 3.575426119359231603 ) ) ;
#14136 = ORIENTED_EDGE ( 'NONE', *, *, #4018, .F. ) ;
#14137 = DIRECTION ( 'NONE',  ( -0.000000000000000000, 1.000000000000000000, 1.734723475976806848E-16 ) ) ;
#14138 = DIRECTION ( 'NONE',  ( -1.000000000000000000, -0.000000000000000000, -0.000000000000000000 ) ) ;
#14139 = LINE ( 'NONE', #1043, #15878 ) ;
#14140 = CARTESIAN_POINT ( 'NONE',  ( 0.3137051932979792457, -12.91601973349266963, -4.679953077377624560 ) ) ;
#14141 = CARTESIAN_POINT ( 'NONE',  ( 1.846138399168762101, 7.646096044339892650, 9.815003036200437236 ) ) ;
#14142 = AXIS2_PLACEMENT_3D ( 'NONE', #5474, #13993, #14277 ) ;
#14143 = ADVANCED_FACE ( 'NONE', ( #11231 ), #10415, .F. ) ;
#14144 = CARTESIAN_POINT ( 'NONE',  ( 0.000000000000000000, 0.000000000000000000, 0.000000000000000000 ) ) ;
#14145 = CARTESIAN_POINT ( 'NONE',  ( 0.4862570985993235340, 0.7479633556564388996, -13.89016912371016765 ) ) ;
#14146 = EDGE_CURVE ( 'NONE', #11242, #16036, #14133, .T. ) ;
#14147 = EDGE_CURVE ( 'NONE', #13349, #5705, #8354, .T. ) ;
#14148 = CIRCLE ( 'NONE', #10813, 1.500000000000000000 ) ;
#14149 = LINE ( 'NONE', #1053, #15003 ) ;
#14151 = VERTEX_POINT ( 'NONE', #2333 ) ;
#14150 = CARTESIAN_POINT ( 'NONE',  ( -194.9999999999999716, 4.999999999999973355, 3.000000000000000000 ) ) ;
#14152 = CARTESIAN_POINT ( 'NONE',  ( 2.636624412716061627, -7.605649742761058540, -14.14563173255469408 ) ) ;
#14153 = CARTESIAN_POINT ( 'NONE',  ( 16.56679352167444819, 0.008252760440870188924, -0.004277682826583317083 ) ) ;
#14154 = CARTESIAN_POINT ( 'NONE',  ( 1.254255976357087521, 11.25336128106905420, 9.426444230096484134 ) ) ;
#14155 = B_SPLINE_CURVE_WITH_KNOTS ( 'NONE', 3,
 ( #5221, #18314, #11062, #16878 ),
 .UNSPECIFIED., .F., .F.,
 ( 4, 4 ),
 ( 4.873469348537302793E-16, 0.002004993803842133101 ),
 .UNSPECIFIED. ) ;
#14156 = ORIENTED_EDGE ( 'NONE', *, *, #11640, .T. ) ;
#14157 = CARTESIAN_POINT ( 'NONE',  ( 1.846138399168762101, -9.815003036200465658, 7.646096044339859787 ) ) ;
#14158 = FACE_OUTER_BOUND ( 'NONE', #17726, .T. ) ;
#14159 = ORIENTED_EDGE ( 'NONE', *, *, #4214, .F. ) ;
#14160 = CARTESIAN_POINT ( 'NONE',  ( 0.3137051932979792457, 4.679953077377485116, 12.91601973349272114 ) ) ;
#14161 = AXIS2_PLACEMENT_3D ( 'NONE', #12887, #4385, #11375 ) ;
#14162 = CARTESIAN_POINT ( 'NONE',  ( 20.00000000000000711, -45.00000000000000000, 3.000000000000000000 ) ) ;
#14163 = CARTESIAN_POINT ( 'NONE',  ( 2.697797270744666687, -8.537712152180933600, 10.19107313879054466 ) ) ;
#14164 = CARTESIAN_POINT ( 'NONE',  ( 0.3137051932979792457, 11.37800749014142276, -7.698472063774345564 ) ) ;
#14165 = CARTESIAN_POINT ( 'NONE',  ( 20.00000000000000711, -39.99999999999999289, 0.000000000000000000 ) ) ;
#14166 = UNCERTAINTY_MEASURE_WITH_UNIT (LENGTH_MEASURE( 1.000000000000000082E-05 ), #7797, 'distance_accuracy_value', 'NONE');
#14167 = VERTEX_POINT ( 'NONE', #1076 ) ;
#14168 = APPLICATION_PROTOCOL_DEFINITION ( 'draft international standard', 'automotive_design', 1998, #826 ) ;
#14169 = B_SPLINE_CURVE_WITH_KNOTS ( 'NONE', 3,
 ( #12533, #3938, #9757, #14154, #5368, #11218 ),
 .UNSPECIFIED., .F., .F.,
 ( 4, 2, 4 ),
 ( 0.000000000000000000, 0.001656992708821599649, 0.003313985417643199299 ),
 .UNSPECIFIED. ) ;
#14170 = DIRECTION ( 'NONE',  ( -0.4246593920385850485, -0.1376957914266803973, 0.8948208031649685923 ) ) ;
#14171 = DIRECTION ( 'NONE',  ( 1.000000000000000000, 1.239088197126290570E-16, -0.000000000000000000 ) ) ;
#14172 = CARTESIAN_POINT ( 'NONE',  ( 1.847380140988743591, -3.949801494731685292, -11.79969976631075390 ) ) ;
#14173 = CARTESIAN_POINT ( 'NONE',  ( 16.56679352167444819, -0.006526964904752395082, 0.006618561353600064395 ) ) ;
#14174 = CARTESIAN_POINT ( 'NONE',  ( 0.3095370825347224519, 3.806662003783413351, 13.20347358821915940 ) ) ;
#14175 = AXIS2_PLACEMENT_3D ( 'NONE', #8460, #2794, #15710 ) ;
#14176 = EDGE_CURVE ( 'NONE', #8361, #3320, #15793, .T. ) ;
#14177 = EDGE_LOOP ( 'NONE', ( #15655, #17579, #16638, #1648 ) ) ;
#14178 = CARTESIAN_POINT ( 'NONE',  ( 0.3150692679895978343, 11.20465057551037091, -7.951395415074959061 ) ) ;
#14179 = CARTESIAN_POINT ( 'NONE',  ( 1.918918678667045130, 6.832809802519163256, -10.48466773720554279 ) ) ;
#14180 = EDGE_CURVE ( 'NONE', #209, #2120, #16654, .T. ) ;
#14181 = ORIENTED_EDGE ( 'NONE', *, *, #4096, .F. ) ;
#14182 = AXIS2_PLACEMENT_3D ( 'NONE', #6905, #3942, #2675 ) ;
#14183 = VERTEX_POINT ( 'NONE', #17134 ) ;
#14184 = ORIENTED_EDGE ( 'NONE', *, *, #2679, .F. ) ;
#14185 = ORIENTED_EDGE ( 'NONE', *, *, #15004, .T. ) ;
#14186 = EDGE_CURVE ( 'NONE', #13031, #14481, #6646, .T. ) ;
#14187 = B_SPLINE_CURVE_WITH_KNOTS ( 'NONE', 3,
 ( #11890, #8733, #1762, #1473, #14562, #1656 ),
 .UNSPECIFIED., .F., .F.,
 ( 4, 2, 4 ),
 ( 3.337089043155729788E-17, 0.0001825746017570573684, 0.0003651492035140813976 ),
 .UNSPECIFIED. ) ;
#14188 = CARTESIAN_POINT ( 'NONE',  ( 1.562796894703937678, 6.799999999999999822, -1.500000000000000000 ) ) ;
#14189 = CARTESIAN_POINT ( 'NONE',  ( 1.977436885026784941, 6.153171729169462090, -14.12046670317587704 ) ) ;
#14190 = AXIS2_PLACEMENT_3D ( 'NONE', #2150, #2323, #7991 ) ;
#14191 = CARTESIAN_POINT ( 'NONE',  ( 3.950837973638675393, 6.888253895133292559, 12.81214529934977797 ) ) ;
#14192 = DIRECTION ( 'NONE',  ( -0.000000000000000000, 0.5000000000000003331, -0.8660254037844384856 ) ) ;
#14193 = AXIS2_PLACEMENT_3D ( 'NONE', #2890, #13039, #5766 ) ;
#14194 = CIRCLE ( 'NONE', #13589, 5.000000000000000000 ) ;
#14195 = LINE ( 'NONE', #12760, #13204 ) ;
#14196 = DIRECTION ( 'NONE',  ( -0.000000000000000000, 1.000000000000000000, 0.000000000000000000 ) ) ;
#14197 = EDGE_CURVE ( 'NONE', #12607, #7783, #13987, .T. ) ;
#14198 = B_SPLINE_CURVE_WITH_KNOTS ( 'NONE', 3,
 ( #16541, #13668, #10615, #580, #3128, #9261 ),
 .UNSPECIFIED., .F., .F.,
 ( 4, 2, 4 ),
 ( 2.790109556687801444E-18, 0.0002017457492448089095, 0.0004034914984896150001 ),
 .UNSPECIFIED. ) ;
#14199 = CARTESIAN_POINT ( 'NONE',  ( 8.522092701127531811, 6.946128462138595694, -0.3779863304871462493 ) ) ;
#14200 = DIRECTION ( 'NONE',  ( 1.000000000000000000, 0.000000000000000000, 0.000000000000000000 ) ) ;
#14201 = VERTEX_POINT ( 'NONE', #4524 ) ;
#14202 = EDGE_CURVE ( 'NONE', #5120, #12310, #13224, .T. ) ;
#14203 = EDGE_CURVE ( 'NONE', #17476, #6505, #14903, .T. ) ;
#14204 =( BOUNDED_SURFACE ( )  B_SPLINE_SURFACE ( 3, 1, ( 
 ( #8001, #12202 ),
 ( #13807, #13627 ),
 ( #10767, #15335 ),
 ( #18027, #6655 ) ),
 .UNSPECIFIED., .F., .F., .T. ) 
 B_SPLINE_SURFACE_WITH_KNOTS ( ( 4, 4 ),
 ( 2, 2 ),
 ( 0.000000000000000000, 1.000000000000000000 ),
 ( 0.000000000000000000, 1.000000000000000000 ),
 .UNSPECIFIED. ) 
 GEOMETRIC_REPRESENTATION_ITEM ( )  RATIONAL_B_SPLINE_SURFACE ( (
 ( 1.000000000000000000, 1.000000000000000000),
 ( 0.7792777138730158093, 0.9689936506012928330),
 ( 0.7792777138730158093, 0.9689936506012928330),
 ( 1.000000000000000000, 1.000000000000000000) ) ) 
 REPRESENTATION_ITEM ( '' )  SURFACE ( )  );
#14205 = VERTEX_POINT ( 'NONE', #222 ) ;
#14206 = ORIENTED_EDGE ( 'NONE', *, *, #4614, .T. ) ;
#14207 = ORIENTED_EDGE ( 'NONE', *, *, #10424, .F. ) ;
#14208 = AXIS2_PLACEMENT_3D ( 'NONE', #11293, #1238, #12711 ) ;
#14209 = VERTEX_POINT ( 'NONE', #1265 ) ;
#14210 = CONICAL_SURFACE ( 'NONE', #1701, 14.54644660717763927, 0.8559913436420816257 ) ;
#14211 = DIRECTION ( 'NONE',  ( -1.000000000000000000, -0.000000000000000000, -0.000000000000000000 ) ) ;
#14212 = CARTESIAN_POINT ( 'NONE',  ( 3.353306896162455697, -13.62210141459498125, 3.007732942432364442 ) ) ;
#14213 = CARTESIAN_POINT ( 'NONE',  ( 16.56753206892534891, -0.008432171035096417550, 0.004368917149005425125 ) ) ;
#14214 = CARTESIAN_POINT ( 'NONE',  ( 0.3137051932979792457, 13.20008686438105983, 3.805684345189833451 ) ) ;
#14215 = FACE_OUTER_BOUND ( 'NONE', #3074, .T. ) ;
#14216 = VERTEX_POINT ( 'NONE', #13116 ) ;
#14217 = CARTESIAN_POINT ( 'NONE',  ( 16.56822296793089322, 0.0007467251401297140970, 0.01011126603341077831 ) ) ;
#14218 = EDGE_CURVE ( 'NONE', #11285, #17875, #10320, .T. ) ;
#14219 = CARTESIAN_POINT ( 'NONE',  ( -4.999999999999995559, -30.00000000000000000, 6.000000000000000000 ) ) ;
#14220 = CARTESIAN_POINT ( 'NONE',  ( 1.824285781649040761, 7.499999999999999112, -15.12168601478843044 ) ) ;
#14221 = CARTESIAN_POINT ( 'NONE',  ( 5.000000000000004441, -27.00000000000000000, 6.000000000000000000 ) ) ;
#14222 = CARTESIAN_POINT ( 'NONE',  ( 2.320521194581858460, 15.43440938316986610, 3.126729093672275805 ) ) ;
#14223 = CARTESIAN_POINT ( 'NONE',  ( 8.522092701127531811, -5.841710761610102942, -3.777034505568587885 ) ) ;
#14224 = CARTESIAN_POINT ( 'NONE',  ( 0.3058872367615230181, -7.578326039752686150, 11.46514199369355325 ) ) ;
#14225 = AXIS2_PLACEMENT_3D ( 'NONE', #18487, #3965, #8188 ) ;
#14226 = DIRECTION ( 'NONE',  ( -1.000000000000000000, -0.000000000000000000, -0.000000000000000000 ) ) ;
#14227 = ORIENTED_EDGE ( 'NONE', *, *, #4799, .T. ) ;
#14229 = EDGE_LOOP ( 'NONE', ( #17916, #18615, #7691, #15254 ) ) ;
#14228 = DIRECTION ( 'NONE',  ( -1.000000000000000000, 0.000000000000000000, 0.000000000000000000 ) ) ;
#14230 = CARTESIAN_POINT ( 'NONE',  ( 0.3307726912345222980, 4.812300915532974344, 12.88561780039860416 ) ) ;
#14231 = DIRECTION ( 'NONE',  ( -1.000000000000000000, 0.000000000000000000, 0.000000000000000000 ) ) ;
#14232 = EDGE_CURVE ( 'NONE', #3195, #9890, #12322, .T. ) ;
#14233 = VERTEX_POINT ( 'NONE', #12923 ) ;
#14234 = CARTESIAN_POINT ( 'NONE',  ( 16.57605080000000086, 3.061616997868383141E-16, -2.500000000000000000 ) ) ;
#14235 = CARTESIAN_POINT ( 'NONE',  ( 1.846822687350019754, -12.43915556955403545, -0.2922081769261452022 ) ) ;
#14236 = CARTESIAN_POINT ( 'NONE',  ( 16.56872352241294521, -0.01033355228142402750, 0.001442253899401767583 ) ) ;
#14237 = COLOUR_RGB ( '', 0.40784314, 0.44705882, 0.49803922) ;
#14238 = CARTESIAN_POINT ( 'NONE',  ( 16.56822296793089322, -0.005339139727952984908, -0.008619100080558656299 ) ) ;
#14239 = ORIENTED_EDGE ( 'NONE', *, *, #6393, .F. ) ;
#14240 = LINE ( 'NONE', #12801, #12648 ) ;
#14241 = ADVANCED_FACE ( 'NONE', ( #15979, #17717 ), #14642, .F. ) ;
#14242 = DIRECTION ( 'NONE',  ( -0.7561779333270775005, -0.1688126975276600938, 0.6322161072786937064 ) ) ;
#14243 = CARTESIAN_POINT ( 'NONE',  ( 0.3148208552358917056, -13.73693263646118901, 0.2299193288886990094 ) ) ;
#14244 = SHAPE_REPRESENTATION ( 'straight miter gear_iso_ISO - Straight miter gear 1.5M20T 20PA 2FW ---20O10H16.576MD10.0S1', ( #2030 ), #8454 ) ;
#14245 =( BOUNDED_SURFACE ( )  B_SPLINE_SURFACE ( 3, 1, ( 
 ( #10722, #500 ),
 ( #3348, #307 ),
 ( #17989, #597 ),
 ( #4895, #12250 ) ),
 .UNSPECIFIED., .F., .F., .T. ) 
 B_SPLINE_SURFACE_WITH_KNOTS ( ( 4, 4 ),
 ( 2, 2 ),
 ( 0.000000000000000000, 1.000000000000000000 ),
 ( 0.000000000000000000, 1.000000000000000000 ),
 .UNSPECIFIED. ) 
 GEOMETRIC_REPRESENTATION_ITEM ( )  RATIONAL_B_SPLINE_SURFACE ( (
 ( 1.000000000000000000, 1.000000000000000000),
 ( 0.9593108457356467333, 0.9995965569486454649),
 ( 0.9593108457356467333, 0.9995965569486454649),
 ( 1.000000000000000000, 1.000000000000000000) ) ) 
 REPRESENTATION_ITEM ( '' )  SURFACE ( )  );
#14246 = CARTESIAN_POINT ( 'NONE',  ( -20.00000000000000000, 0.000000000000000000, -16.99999999999999645 ) ) ;
#14247 = CARTESIAN_POINT ( 'NONE',  ( -2.500000000000000000, 3.061616997868383141E-16, -3.000000000000000000 ) ) ;
#14248 = AXIS2_PLACEMENT_3D ( 'NONE', #5248, #15561, #2378 ) ;
#14249 = VECTOR ( 'NONE', #5313, 1000.000000000000000 ) ;
#14250 = AXIS2_PLACEMENT_3D ( 'NONE', #6079, #14765, #13431 ) ;
#14251 = CARTESIAN_POINT ( 'NONE',  ( 1.977228804423231345, 7.806978995470744032, -13.27756617201399969 ) ) ;
#14252 = AXIS2_PLACEMENT_3D ( 'NONE', #18825, #13545, #11926 ) ;
#14253 = CARTESIAN_POINT ( 'NONE',  ( 1.562796894703937678, 0.000000000000000000, 0.000000000000000000 ) ) ;
#14255 = EDGE_LOOP ( 'NONE', ( #9828, #2254, #6579, #11794 ) ) ;
#14254 = CARTESIAN_POINT ( 'NONE',  ( 16.57210152137263393, -0.01453130299868639515, 0.0006600038696349324685 ) ) ;
#14256 = CARTESIAN_POINT ( 'NONE',  ( 16.56872352241294521, -0.004907101719994693724, 0.009207754980063731845 ) ) ;
#14257 = VECTOR ( 'NONE', #10725, 1000.000000000000000 ) ;
#14258 = CARTESIAN_POINT ( 'NONE',  ( 5.000000000000000888, 17.00000000000000000, 7.000000000000000000 ) ) ;
#14259 = ORIENTED_EDGE ( 'NONE', *, *, #18693, .F. ) ;
#14260 = CARTESIAN_POINT ( 'NONE',  ( 0.4754618798421162973, -5.007009103465343003, 12.98792082933642789 ) ) ;
#14261 = AXIS2_PLACEMENT_3D ( 'NONE', #1854, #9015, #6056 ) ;
#14262 = CARTESIAN_POINT ( 'NONE',  ( 1.845756295923357326, 12.43231724724606835, -0.4783934145702458673 ) ) ;
#14263 = ORIENTED_EDGE ( 'NONE', *, *, #15156, .F. ) ;
#14264 = AXIS2_PLACEMENT_3D ( 'NONE', #17702, #8988, #14816 ) ;
#14265 = CARTESIAN_POINT ( 'NONE',  ( 0.3137051932979757485, -8.442169467526770887, -10.83767969834812561 ) ) ;
#14266 = ADVANCED_FACE ( 'NONE', ( #13207 ), #6672, .T. ) ;
#14267 = ADVANCED_FACE ( 'NONE', ( #16177 ), #5644, .F. ) ;
#14268 = ADVANCED_FACE ( 'NONE', ( #121 ), #11783, .T. ) ;
#14269 = LINE ( 'NONE', #7197, #17997 ) ;
#14270 = LINE ( 'NONE', #1169, #4749 ) ;
#14271 = DIRECTION ( 'NONE',  ( -0.000000000000000000, -0.000000000000000000, -1.000000000000000000 ) ) ;
#14272 = ORIENTED_EDGE ( 'NONE', *, *, #12367, .T. ) ;
#14273 = VECTOR ( 'NONE', #14171, 1000.000000000000000 ) ;
#14274 = CARTESIAN_POINT ( 'NONE',  ( 1.104287921197080512E-14, -7.013167318348350499, 25.01316734529528674 ) ) ;
#14275 = CARTESIAN_POINT ( 'NONE',  ( 1.959212340397967766, -0.6675998551412658522, 12.53706137681888677 ) ) ;
#14276 = ADVANCED_FACE ( 'NONE', ( #11596 ), #554, .F. ) ;
#14277 = DIRECTION ( 'NONE',  ( 0.000000000000000000, 0.000000000000000000, 1.000000000000000000 ) ) ;
#14278 = CARTESIAN_POINT ( 'NONE',  ( 2.636624412715093513, -14.14563173255330142, 7.605649742761597665 ) ) ;
#14279 = CARTESIAN_POINT ( 'NONE',  ( 16.56822296793089322, -0.005339139727952984908, -0.008619100080558656299 ) ) ;
#14280 = ORIENTED_EDGE ( 'NONE', *, *, #5610, .F. ) ;
#14281 = CARTESIAN_POINT ( 'NONE',  ( 2.636624412715435462, -15.80357026013316712, -2.862162146983298516 ) ) ;
#14282 = CARTESIAN_POINT ( 'NONE',  ( 2.002547531651519996, -7.942910686618100513, -9.778737580845787036 ) ) ;
#14283 = VERTEX_POINT ( 'NONE', #1462 ) ;
#14284 = ORIENTED_EDGE ( 'NONE', *, *, #3436, .F. ) ;
#14285 = ORIENTED_EDGE ( 'NONE', *, *, #7158, .T. ) ;
#14286 = DIRECTION ( 'NONE',  ( -1.000000000000000000, -0.000000000000000000, -0.000000000000000000 ) ) ;
#14287 = VERTEX_POINT ( 'NONE', #7300 ) ;
#14288 = CONICAL_SURFACE ( 'NONE', #16995, 14.54644660717763927, 0.8559913436420816257 ) ;
#14289 = DIRECTION ( 'NONE',  ( 0.000000000000000000, 0.000000000000000000, 1.000000000000000000 ) ) ;
#14290 = EDGE_CURVE ( 'NONE', #9252, #4800, #15722, .T. ) ;
#14291 = CARTESIAN_POINT ( 'NONE',  ( 0.3137051932979757485, -4.679953077377398074, -12.91601973349275134 ) ) ;
#14292 = EDGE_CURVE ( 'NONE', #13464, #18846, #2199, .T. ) ;
#14293 = CARTESIAN_POINT ( 'NONE',  ( 8.522092701127531811, 6.722964936702098271, 1.786985377232055860 ) ) ;
#14294 = CARTESIAN_POINT ( 'NONE',  ( 16.57778382496167424, -0.01092721432669101385, 0.01018821665058845458 ) ) ;
#14295 = AXIS2_PLACEMENT_3D ( 'NONE', #6904, #10943, #2146 ) ;
#14296 = PRESENTATION_STYLE_ASSIGNMENT (( #15814 ) ) ;
#14297 = DIRECTION ( 'NONE',  ( 0.000000000000000000, 0.000000000000000000, 1.000000000000000000 ) ) ;
#14298 = CARTESIAN_POINT ( 'NONE',  ( 2.002547531651519996, 10.57595306287302250, -6.845637710436074386 ) ) ;
#14299 = CARTESIAN_POINT ( 'NONE',  ( 16.56872352241294521, -0.001821578298043862289, 0.01027347319884366027 ) ) ;
#14300 = DIRECTION ( 'NONE',  ( -1.000000000000000000, -0.000000000000000000, -0.000000000000000000 ) ) ;
#14301 = EDGE_CURVE ( 'NONE', #14216, #10086, #4812, .T. ) ;
#14302 = EDGE_LOOP ( 'NONE', ( #17728, #1996, #13770, #8562 ) ) ;
#14303 = VERTEX_POINT ( 'NONE', #18254 ) ;
#14304 = ORIENTED_EDGE ( 'NONE', *, *, #1941, .T. ) ;
#14305 = ORIENTED_EDGE ( 'NONE', *, *, #9502, .F. ) ;
#14306 = PLANE ( 'NONE',  #2868 ) ;
#14307 = CARTESIAN_POINT ( 'NONE',  ( 2.697797270744668019, -12.89731672021093090, 3.226410068829379973 ) ) ;
#14308 = CARTESIAN_POINT ( 'NONE',  ( 3.074695600508242421, -2.093687500613561348, -15.41438262616270194 ) ) ;
#14309 = EDGE_LOOP ( 'NONE', ( #7494, #13372, #9531, #8160 ) ) ;
#14310 = DIRECTION ( 'NONE',  ( 0.000000000000000000, 0.000000000000000000, -1.000000000000000000 ) ) ;
#14311 = CARTESIAN_POINT ( 'NONE',  ( 0.4384471787762818096, 0.7363690479466327155, 13.84291427302852462 ) ) ;
#14312 = EDGE_CURVE ( 'NONE', #3136, #13361, #9198, .T. ) ;
#14313 = CARTESIAN_POINT ( 'NONE',  ( 2.061733300930400858, 7.499999999999732658, -13.14107379030440370 ) ) ;
#14314 = CARTESIAN_POINT ( 'NONE',  ( 16.56822296793089322, -0.008619100080559813359, -0.005339139727952636229 ) ) ;
#14315 = STYLED_ITEM ( 'NONE', ( #13984 ), #16760 ) ;
#14316 = CARTESIAN_POINT ( 'NONE',  ( 3.950837973638668288, 0.000000000000000000, 0.000000000000000000 ) ) ;
#14317 = CARTESIAN_POINT ( 'NONE',  ( 0.000000000000000000, 0.000000000000000000, 0.000000000000000000 ) ) ;
#14318 = DIRECTION ( 'NONE',  ( 0.000000000000000000, -0.000000000000000000, -1.000000000000000000 ) ) ;
#14319 =( BOUNDED_SURFACE ( )  B_SPLINE_SURFACE ( 3, 1, ( 
 ( #13825, #8198 ),
 ( #15076, #923 ),
 ( #1995, #7833 ),
 ( #13653, #6391 ) ),
 .UNSPECIFIED., .F., .F., .T. ) 
 B_SPLINE_SURFACE_WITH_KNOTS ( ( 4, 4 ),
 ( 2, 2 ),
 ( 0.000000000000000000, 1.000000000000000000 ),
 ( 0.000000000000000000, 1.000000000000000000 ),
 .UNSPECIFIED. ) 
 GEOMETRIC_REPRESENTATION_ITEM ( )  RATIONAL_B_SPLINE_SURFACE ( (
 ( 1.000000000000000000, 1.000000000000000000),
 ( 0.7792777138730160313, 0.9689936506012927220),
 ( 0.7792777138730160313, 0.9689936506012927220),
 ( 1.000000000000000000, 1.000000000000000000) ) ) 
 REPRESENTATION_ITEM ( '' )  SURFACE ( )  );
#14320 = DIRECTION ( 'NONE',  ( -0.000000000000000000, -1.000000000000000000, -0.000000000000000000 ) ) ;
#14321 = ORIENTED_EDGE ( 'NONE', *, *, #10831, .F. ) ;
#14323 = ORIENTED_EDGE ( 'NONE', *, *, #15042, .T. ) ;
#14322 = CYLINDRICAL_SURFACE ( 'NONE', #12713, 4.000000000000000000 ) ;
#14324 = CARTESIAN_POINT ( 'NONE',  ( 16.56782317627811096, -0.003357783021327304974, 0.009228812961909584403 ) ) ;
#14325 = EDGE_CURVE ( 'NONE', #1370, #13362, #5697, .T. ) ;
#14326 = CIRCLE ( 'NONE', #8828, 2.499999999999992006 ) ;
#14327 = CARTESIAN_POINT ( 'NONE',  ( 0.3095370825347233956, -13.20347358821911854, -3.806662003783550574 ) ) ;
#14328 = ORIENTED_EDGE ( 'NONE', *, *, #3042, .T. ) ;
#14329 = DIRECTION ( 'NONE',  ( 0.000000000000000000, 1.000000000000000000, 0.000000000000000000 ) ) ;
#14330 = CARTESIAN_POINT ( 'NONE',  ( 15.00000000000000711, -14.99999999999999645, 7.000000000000000000 ) ) ;
#14331 = CARTESIAN_POINT ( 'NONE',  ( 1.918918678667048461, -12.08296592096905187, -3.258447776119960615 ) ) ;
#14332 = ORIENTED_EDGE ( 'NONE', *, *, #747, .T. ) ;
#14333 = CARTESIAN_POINT ( 'NONE',  ( 16.56753206892534891, -0.006669401563385243120, -0.006760771273035091553 ) ) ;
#14334 = LINE ( 'NONE', #10125, #5759 ) ;
#14335 = DIRECTION ( 'NONE',  ( -1.000000000000000000, 0.000000000000000000, -0.000000000000000000 ) ) ;
#14336 = CARTESIAN_POINT ( 'NONE',  ( 0.3151926232592464627, -13.09050869763090219, -4.172630140040936908 ) ) ;
#14337 = LINE ( 'NONE', #18720, #11153 ) ;
#14338 = EDGE_CURVE ( 'NONE', #2787, #2558, #254, .T. ) ;
#14339 = CARTESIAN_POINT ( 'NONE',  ( -5.000000000000000000, 6.123233995736766282E-16, 0.000000000000000000 ) ) ;
#14340 = CARTESIAN_POINT ( 'NONE',  ( 0.4754618798421167414, 3.583352865732670534, 13.45049478164061263 ) ) ;
#14342 = ORIENTED_EDGE ( 'NONE', *, *, #14301, .T. ) ;
#14341 = DIRECTION ( 'NONE',  ( 1.540743955509788340E-33, 1.000000000000000000, 2.533398541561209262E-17 ) ) ;
#14343 = CARTESIAN_POINT ( 'NONE',  ( 0.4862570985993235340, -8.769551628660812170, 10.79774104611370333 ) ) ;
#14344 = ORIENTED_EDGE ( 'NONE', *, *, #16255, .T. ) ;
#14345 = CARTESIAN_POINT ( 'NONE',  ( 2.320521194582656932, -14.32454473829943886, 6.542541239685230714 ) ) ;
#14346 = VERTEX_POINT ( 'NONE', #16906 ) ;
#14347 = CARTESIAN_POINT ( 'NONE',  ( 1.847412631396505356, 10.04119192206686328, 7.348689888531877656 ) ) ;
#14348 = SPHERICAL_SURFACE ( 'NONE', #5329, 5.315148208181397216 ) ;
#14349 =( BOUNDED_SURFACE ( )  B_SPLINE_SURFACE ( 3, 1, ( 
 ( #2631, #16101 ),
 ( #2983, #11264 ),
 ( #3075, #5501 ),
 ( #9800, #14564 ) ),
 .UNSPECIFIED., .F., .F., .T. ) 
 B_SPLINE_SURFACE_WITH_KNOTS ( ( 4, 4 ),
 ( 2, 2 ),
 ( 0.000000000000000000, 1.000000000000000000 ),
 ( 0.000000000000000000, 1.000000000000000000 ),
 .UNSPECIFIED. ) 
 GEOMETRIC_REPRESENTATION_ITEM ( )  RATIONAL_B_SPLINE_SURFACE ( (
 ( 1.000000000000000000, 1.000000000000000000),
 ( 0.9933953342250438912, 0.8357391271907739227),
 ( 0.9933953342250438912, 0.8357391271907739227),
 ( 1.000000000000000000, 1.000000000000000000) ) ) 
 REPRESENTATION_ITEM ( '' )  SURFACE ( )  );
#14350 = ORIENTED_EDGE ( 'NONE', *, *, #9332, .T. ) ;
#14351 = VECTOR ( 'NONE', #17805, 1000.000000000000000 ) ;
#14352 = CARTESIAN_POINT ( 'NONE',  ( 0.3132635586635994507, -3.740017578711855695, 13.21855946425835882 ) ) ;
#14353 = CARTESIAN_POINT ( 'NONE',  ( 0.3145729642390390768, -10.93201268464378373, 8.321438378985218876 ) ) ;
#14354 = CARTESIAN_POINT ( 'NONE',  ( 1.560000000000000053, -0.8660254037844384856, 1.500000000000000000 ) ) ;
#14355 = VERTEX_POINT ( 'NONE', #9107 ) ;
#14356 = ITEM_DEFINED_TRANSFORMATION ( 'NONE', 'NONE', #2935,  #2030 ) ;
#14357 = DIRECTION ( 'NONE',  ( -1.000000000000000000, 0.000000000000000000, 0.000000000000000000 ) ) ;
#14358 = DIRECTION ( 'NONE',  ( 0.000000000000000000, -0.000000000000000000, 1.000000000000000000 ) ) ;
#14359 = LINE ( 'NONE', #11321, #11712 ) ;
#14360 = CARTESIAN_POINT ( 'NONE',  ( 2.002547531651519996, 9.778737580845815458, -7.942910686618064986 ) ) ;
#14361 = CARTESIAN_POINT ( 'NONE',  ( -27.50000000000000711, -12.50000000000000178, 6.000000000000000000 ) ) ;
#14362 = EDGE_CURVE ( 'NONE', #13344, #3494, #11184, .T. ) ;
#14363 = ORIENTED_EDGE ( 'NONE', *, *, #8264, .F. ) ;
#14364 = CARTESIAN_POINT ( 'NONE',  ( 8.522092701127531811, 3.777034505568607425, -5.841710761610089619 ) ) ;
#14365 = CARTESIAN_POINT ( 'NONE',  ( 1.959283090834841090, -7.909254450748933962, -9.750336807931228478 ) ) ;
#14366 = EDGE_LOOP ( 'NONE', ( #9736, #2200, #611, #12563 ) ) ;
#14367 = VERTEX_POINT ( 'NONE', #8223 ) ;
#14369 = CARTESIAN_POINT ( 'NONE',  ( 1.847426409206446518, -0.01438352405999345808, 12.44303504652078018 ) ) ;
#14368 = VECTOR ( 'NONE', #7445, 1000.000000000000114 ) ;
#14370 = VERTEX_POINT ( 'NONE', #9009 ) ;
#14371 = CARTESIAN_POINT ( 'NONE',  ( 16.56753206892534891, 0.001549402974394163733, 0.009369540855502535986 ) ) ;
#14372 = ORIENTED_EDGE ( 'NONE', *, *, #5905, .F. ) ;
#14373 = CARTESIAN_POINT ( 'NONE',  ( 3.950837973638668288, 0.000000000000000000, 0.000000000000000000 ) ) ;
#14374 = CARTESIAN_POINT ( 'NONE',  ( 1.846524061778019199, -9.853584647934329865, -7.597197846158187495 ) ) ;
#14375 = APPLICATION_CONTEXT ( 'automotive_design' ) ;
#14376 = CARTESIAN_POINT ( 'NONE',  ( 16.56822296793089322, 0.003834730849371879857, 0.009385634690642069913 ) ) ;
#14377 = CARTESIAN_POINT ( 'NONE',  ( 1.846138399168762989, 4.238866729160403857, 11.69739621335923729 ) ) ;
#14378 =( LENGTH_UNIT ( ) NAMED_UNIT ( * ) SI_UNIT ( .MILLI., .METRE. ) );
#14379 = CARTESIAN_POINT ( 'NONE',  ( 3.686287386450715076E-15, -16.60000000000000142, 25.01316734529526187 ) ) ;
#14380 = AXIS2_PLACEMENT_3D ( 'NONE', #6, #17490, #1341 ) ;
#14381 = LINE ( 'NONE', #5407, #16116 ) ;
#14382 = CARTESIAN_POINT ( 'NONE',  ( 1.342453679581834924, 9.456403821038962931, -11.38190519890843255 ) ) ;
#14383 = ADVANCED_FACE ( 'NONE', ( #11091 ), #1157, .F. ) ;
#14384 = EDGE_CURVE ( 'NONE', #8099, #3320, #3652, .T. ) ;
#14385 = ORIENTED_EDGE ( 'NONE', *, *, #14897, .F. ) ;
#14386 = EDGE_CURVE ( 'NONE', #7547, #2319, #18248, .T. ) ;
#14387 = ORIENTED_EDGE ( 'NONE', *, *, #1285, .T. ) ;
#14388 = ORIENTED_EDGE ( 'NONE', *, *, #16460, .F. ) ;
#14389 = VERTEX_POINT ( 'NONE', #2375 ) ;
#14390 = VERTEX_POINT ( 'NONE', #17905 ) ;
#14391 = B_SPLINE_CURVE_WITH_KNOTS ( 'NONE', 3,
 ( #7418, #4261, #11903, #11614, #16109, #1386 ),
 .UNSPECIFIED., .F., .F.,
 ( 4, 2, 4 ),
 ( 4.003426615173598157E-17, 0.0002014099069817276190, 0.0004028198139634152309 ),
 .UNSPECIFIED. ) ;
#14392 = FACE_OUTER_BOUND ( 'NONE', #16184, .T. ) ;
#14393 = CARTESIAN_POINT ( 'NONE',  ( 0.3095370825347224519, 13.73357284481724783, -0.4597470195090672673 ) ) ;
#14394 = CARTESIAN_POINT ( 'NONE',  ( 0.3145729642390366343, 7.825496023201474749, -11.29233589755984113 ) ) ;
#14395 = ORIENTED_EDGE ( 'NONE', *, *, #1515, .F. ) ;
#14396 = CARTESIAN_POINT ( 'NONE',  ( 16.58200780006414732, -0.009393638146079803797, 0.006043560077721671885 ) ) ;
#14397 = CARTESIAN_POINT ( 'NONE',  ( 4.525831033741626541, 7.500000000000000000, -13.14978481913310304 ) ) ;
#14398 = DIRECTION ( 'NONE',  ( -0.000000000000000000, -0.000000000000000000, 1.000000000000000000 ) ) ;
#14399 = DIRECTION ( 'NONE',  ( -0.000000000000000000, 0.000000000000000000, 1.000000000000000000 ) ) ;
#14400 = CARTESIAN_POINT ( 'NONE',  ( 2.002547531651519996, -10.57595306287296921, 6.845637710436153434 ) ) ;
#14401 = CARTESIAN_POINT ( 'NONE',  ( 0.3095370825347233956, -7.700448427571951804, 11.38092634279625948 ) ) ;
#14402 = B_SPLINE_CURVE_WITH_KNOTS ( 'NONE', 3,
 ( #3451, #8238, #10927, #18085, #2126, #4985 ),
 .UNSPECIFIED., .F., .F.,
 ( 4, 2, 4 ),
 ( 3.522439207679730663E-17, 0.0001825746017570575039, 0.0003651492035140797713 ),
 .UNSPECIFIED. ) ;
#14403 = CARTESIAN_POINT ( 'NONE',  ( -194.9999999999999716, -45.00000000000003553, 3.000000000000000000 ) ) ;
#14404 = ORIENTED_EDGE ( 'NONE', *, *, #16792, .T. ) ;
#14405 = VERTEX_POINT ( 'NONE', #17006 ) ;
#14406 = CARTESIAN_POINT ( 'NONE',  ( 16.56753206892534891, -0.004253784598196239108, 0.008490833999798910042 ) ) ;
#14407 = ORIENTED_EDGE ( 'NONE', *, *, #85, .T. ) ;
#14408 = EDGE_CURVE ( 'NONE', #6395, #17499, #13375, .T. ) ;
#14409 = ORIENTED_EDGE ( 'NONE', *, *, #14557, .T. ) ;
#14410 = CARTESIAN_POINT ( 'NONE',  ( 1.959212340397916030, 9.750290364083625150, 7.909199412631181758 ) ) ;
#14411 = EDGE_LOOP ( 'NONE', ( #1702, #17709, #3655, #18122 ) ) ;
#14412 = CARTESIAN_POINT ( 'NONE',  ( -1.500000000000001332, 6.799999999999999822, 7.000000000000000000 ) ) ;
#14413 = DIRECTION ( 'NONE',  ( 1.000000000000000000, 0.000000000000000000, 0.000000000000000000 ) ) ;
#14414 = FACE_OUTER_BOUND ( 'NONE', #7649, .T. ) ;
#14415 = CARTESIAN_POINT ( 'NONE',  ( 16.57210152137263393, 0.005118120558001911478, 0.01361613799508963087 ) ) ;
#14416 = VERTEX_POINT ( 'NONE', #11974 ) ;
#14417 = CARTESIAN_POINT ( 'NONE',  ( 8.522092701127531811, 6.946128462138595694, 0.3779863304871469154 ) ) ;
#14418 = VECTOR ( 'NONE', #856, 1000.000000000000000 ) ;
#14419 = DIRECTION ( 'NONE',  ( -1.000000000000000000, -0.000000000000000000, -0.000000000000000000 ) ) ;
#14420 = B_SPLINE_CURVE_WITH_KNOTS ( 'NONE', 3,
 ( #16040, #4294, #2656, #12885, #15753, #1424 ),
 .UNSPECIFIED., .F., .F.,
 ( 4, 2, 4 ),
 ( 4.003426615173598157E-17, 0.0002014099069817276190, 0.0004028198139634152309 ),
 .UNSPECIFIED. ) ;
#14421 = CARTESIAN_POINT ( 'NONE',  ( 0.3148213771069381384, -13.73693585713733611, -0.2297580318216151940 ) ) ;
#14422 = DIRECTION ( 'NONE',  ( 0.000000000000000000, 1.000000000000000000, 0.000000000000000000 ) ) ;
#14423 = B_SPLINE_CURVE_WITH_KNOTS ( 'NONE', 3,
 ( #9755, #17033, #16841, #15583, #2310, #2482 ),
 .UNSPECIFIED., .F., .F.,
 ( 4, 2, 4 ),
 ( 0.000000000000000000, 0.001657017934712276541, 0.003314035869424553082 ),
 .UNSPECIFIED. ) ;
#14424 =( BOUNDED_SURFACE ( )  B_SPLINE_SURFACE ( 3, 1, ( 
 ( #1225, #5520 ),
 ( #11371, #17185 ),
 ( #4101, #9921 ),
 ( #11006, #5436 ) ),
 .UNSPECIFIED., .F., .F., .T. ) 
 B_SPLINE_SURFACE_WITH_KNOTS ( ( 4, 4 ),
 ( 2, 2 ),
 ( 0.000000000000000000, 1.000000000000000000 ),
 ( 0.000000000000000000, 1.000000000000000000 ),
 .UNSPECIFIED. ) 
 GEOMETRIC_REPRESENTATION_ITEM ( )  RATIONAL_B_SPLINE_SURFACE ( (
 ( 1.000000000000000000, 1.000000000000000000),
 ( 0.9933953342250438912, 0.8357391271907739227),
 ( 0.9933953342250438912, 0.8357391271907739227),
 ( 1.000000000000000000, 1.000000000000000000) ) ) 
 REPRESENTATION_ITEM ( '' )  SURFACE ( )  );
#14425 = CARTESIAN_POINT ( 'NONE',  ( 0.4862570985993252548, -3.580942890621766406, 13.44146924561379741 ) ) ;
#14426 = CARTESIAN_POINT ( 'NONE',  ( -112.9592833967653149, -82.42962774651277869, -85.91158569379400944 ) ) ;
#14427 = DIRECTION ( 'NONE',  ( 0.000000000000000000, 0.000000000000000000, 1.000000000000000000 ) ) ;
#14428 = CARTESIAN_POINT ( 'NONE',  ( 2.750000000000000000, 0.000000000000000000, 0.000000000000000000 ) ) ;
#14429 = VERTEX_POINT ( 'NONE', #4713 ) ;
#14430 = PRODUCT_DEFINITION ( 'UNKNOWN', '', #9874, #9242 ) ;
#14431 = EDGE_CURVE ( 'NONE', #16551, #15433, #574, .T. ) ;
#14432 = CARTESIAN_POINT ( 'NONE',  ( 3.950837973638677170, 10.51028938476232355, -10.05648675950114956 ) ) ;
#14434 = ORIENTED_EDGE ( 'NONE', *, *, #17191, .T. ) ;
#14433 = PLANE ( 'NONE',  #11508 ) ;
#14435 = CARTESIAN_POINT ( 'NONE',  ( 0.3170788640506440603, 0.1533108587038062576, -13.74111462631963398 ) ) ;
#14436 = CIRCLE ( 'NONE', #409, 2.055000000000000160 ) ;
#14437 = EDGE_CURVE ( 'NONE', #322, #9741, #11850, .T. ) ;
#14438 = CARTESIAN_POINT ( 'NONE',  ( 0.3095370825347224519, -13.20347358821917183, 3.806662003783363613 ) ) ;
#14439 = EDGE_LOOP ( 'NONE', ( #5777, #7487, #3022, #16415 ) ) ;
#14440 = CARTESIAN_POINT ( 'NONE',  ( 1.846822687350021974, 9.891732594446578375, 7.547953575784160485 ) ) ;
#14441 = CARTESIAN_POINT ( 'NONE',  ( 0.4862570985993252548, 10.79774104611373353, 8.769551628660776643 ) ) ;
#14442 = ORIENTED_EDGE ( 'NONE', *, *, #16232, .T. ) ;
#14443 = CYLINDRICAL_SURFACE ( 'NONE', #12724, 2.500000000000000000 ) ;
#14444 = CARTESIAN_POINT ( 'NONE',  ( 16.56872352241294521, 0.01033355228142499721, 0.001442253899401261912 ) ) ;
#14445 = CARTESIAN_POINT ( 'NONE',  ( 0.3137051932979809665, 3.805684345189785933, 13.20008686438107581 ) ) ;
#14446 = PLANE ( 'NONE',  #16013 ) ;
#14447 = FACE_OUTER_BOUND ( 'NONE', #7677, .T. ) ;
#14448 = VECTOR ( 'NONE', #12484, 1000.000000000000000 ) ;
#14449 = EDGE_CURVE ( 'NONE', #16063, #12518, #16053, .T. ) ;
#14450 = PRESENTATION_STYLE_ASSIGNMENT (( #16081 ) ) ;
#14451 = CARTESIAN_POINT ( 'NONE',  ( 16.56872352241294521, -0.004564908236400030961, 0.009382111268607351909 ) ) ;
#14452 = CARTESIAN_POINT ( 'NONE',  ( 2.636624412714237309, 7.605649742761960042, 14.14563173255213613 ) ) ;
#14453 = CARTESIAN_POINT ( 'NONE',  ( 0.3095370825347233956, -13.20347358821911854, -3.806662003783550574 ) ) ;
#14454 = DIRECTION ( 'NONE',  ( 0.000000000000000000, 0.000000000000000000, 1.000000000000000000 ) ) ;
#14455 = CARTESIAN_POINT ( 'NONE',  ( 2.697797270744668019, -7.053988368581781465, -11.26906156738834675 ) ) ;
#14456 = VERTEX_POINT ( 'NONE', #8308 ) ;
#14457 = CARTESIAN_POINT ( 'NONE',  ( 16.56872352241294521, 0.009382111268606257298, -0.004564908236400254740 ) ) ;
#14458 = CARTESIAN_POINT ( 'NONE',  ( 16.56753206892534891, 0.001549402974393146101, -0.009369540855502138735 ) ) ;
#14459 = ORIENTED_EDGE ( 'NONE', *, *, #15921, .T. ) ;
#14460 = EDGE_LOOP ( 'NONE', ( #10981, #5412, #2230, #3848 ) ) ;
#14461 = CARTESIAN_POINT ( 'NONE',  ( 2.320520222537543198, -15.43440824796705613, 3.126729907239071959 ) ) ;
#14462 = STYLED_ITEM ( 'NONE', ( #387 ), #10437 ) ;
#14463 = VERTEX_POINT ( 'NONE', #14403 ) ;
#14464 = FACE_OUTER_BOUND ( 'NONE', #12906, .T. ) ;
#14465 = VERTEX_POINT ( 'NONE', #8492 ) ;
#14466 = CARTESIAN_POINT ( 'NONE',  ( 0.3132635586635996727, 13.21855946425836592, 3.740017578711807289 ) ) ;
#14467 = CARTESIAN_POINT ( 'NONE',  ( 6.538348415311010520, 2.499999999999998668, -17.00000000000000000 ) ) ;
#14468 = EDGE_CURVE ( 'NONE', #1087, #11886, #6048, .T. ) ;
#14469 = FACE_OUTER_BOUND ( 'NONE', #3817, .T. ) ;
#14470 = CARTESIAN_POINT ( 'NONE',  ( 16.56753206892534891, -0.004368917149004301892, 0.008432171035096367243 ) ) ;
#14471 =( NAMED_UNIT ( * ) SI_UNIT ( $, .STERADIAN. ) SOLID_ANGLE_UNIT ( ) );
#14472 = CARTESIAN_POINT ( 'NONE',  ( 0.8740764193767192047, -0.8420116711622469552, 14.27348595579779911 ) ) ;
#14473 = DIRECTION ( 'NONE',  ( 0.000000000000000000, 0.000000000000000000, 1.000000000000000000 ) ) ;
#14474 = VECTOR ( 'NONE', #11961, 1000.000000000000000 ) ;
#14475 = CARTESIAN_POINT ( 'NONE',  ( 0.3145729642390355241, -12.96842777670210189, 4.535980493005037140 ) ) ;
#14476 = AXIS2_PLACEMENT_3D ( 'NONE', #15944, #8786, #2933 ) ;
#14477 = CARTESIAN_POINT ( 'NONE',  ( 3.950837973638668288, 0.000000000000000000, 0.000000000000000000 ) ) ;
#14478 = EDGE_LOOP ( 'NONE', ( #9448, #7648, #12059, #6485 ) ) ;
#14479 = CIRCLE ( 'NONE', #15109, 14.54644660717763927 ) ;
#14480 = ORIENTED_EDGE ( 'NONE', *, *, #5004, .F. ) ;
#14481 = VERTEX_POINT ( 'NONE', #12874 ) ;
#14482 = ORIENTED_EDGE ( 'NONE', *, *, #7744, .F. ) ;
#14483 = VERTEX_POINT ( 'NONE', #9732 ) ;
#14484 = DIRECTION ( 'NONE',  ( 1.000000000000000000, 0.000000000000000000, -0.000000000000000000 ) ) ;
#14485 = APPLICATION_CONTEXT ( 'automotive_design' ) ;
#14486 = CIRCLE ( 'NONE', #6267, 14.54644660717763927 ) ;
#14487 = CARTESIAN_POINT ( 'NONE',  ( 1.918918678667071775, -0.6348738215464356793, -12.49849921341423986 ) ) ;
#14488 = CARTESIAN_POINT ( 'NONE',  ( 0.3137051932979792457, 8.442169467527008919, -10.83767969834794087 ) ) ;
#14489 = ORIENTED_EDGE ( 'NONE', *, *, #15204, .F. ) ;
#14490 = DIRECTION ( 'NONE',  ( 0.4246593920385849930, 0.1376957914266804250, -0.8948208031649685923 ) ) ;
#14491 = AXIS2_PLACEMENT_3D ( 'NONE', #11723, #10188, #7531 ) ;
#14492 = ADVANCED_FACE ( 'NONE', ( #5512 ), #10004, .T. ) ;
#14493 = EDGE_CURVE ( 'NONE', #8310, #12927, #17272, .T. ) ;
#14494 = FACE_OUTER_BOUND ( 'NONE', #10606, .T. ) ;
#14495 = EDGE_CURVE ( 'NONE', #2604, #5275, #2732, .T. ) ;
#14496 = CARTESIAN_POINT ( 'NONE',  ( 1.861706995891668326, -3.332865258614060355, 12.00328602385079257 ) ) ;
#14497 = CARTESIAN_POINT ( 'NONE',  ( 2.636624412715137478, -2.862162146983530775, 15.80357026013314048 ) ) ;
#14498 = CARTESIAN_POINT ( 'NONE',  ( 16.56753206892534891, -0.006760771273036220858, -0.006669401563384898778 ) ) ;
#14499 = CARTESIAN_POINT ( 'NONE',  ( 2.636624412715093513, -14.14563173255330142, 7.605649742761597665 ) ) ;
#14500 = CARTESIAN_POINT ( 'NONE',  ( 1.845755665168035575, 9.776700214454821847, 7.694641135843453661 ) ) ;
#14501 = CARTESIAN_POINT ( 'NONE',  ( 0.3137051932979757485, -7.698472063774552510, 11.37800749014128421 ) ) ;
#14502 = CARTESIAN_POINT ( 'NONE',  ( -3.335251384444446021, -19.99999999999999645, 6.000000000000000000 ) ) ;
#14503 = ORIENTED_EDGE ( 'NONE', *, *, #6315, .T. ) ;
#14504 = AXIS2_PLACEMENT_3D ( 'NONE', #11475, #7174, #14058 ) ;
#14505 = EDGE_CURVE ( 'NONE', #1807, #14283, #15644, .T. ) ;
#14506 = EDGE_LOOP ( 'NONE', ( #1294, #9956, #1679, #9090 ) ) ;
#14507 = ORIENTED_EDGE ( 'NONE', *, *, #14652, .F. ) ;
#14508 = ORIENTED_EDGE ( 'NONE', *, *, #10454, .T. ) ;
#14509 = DIRECTION ( 'NONE',  ( -1.000000000000000000, -0.000000000000000000, -0.000000000000000000 ) ) ;
#14510 = ORIENTED_EDGE ( 'NONE', *, *, #16024, .T. ) ;
#14511 = CARTESIAN_POINT ( 'NONE',  ( 2.353870697619111496, 3.268530966681629568, 12.53036919722785925 ) ) ;
#14512 = FACE_OUTER_BOUND ( 'NONE', #13104, .T. ) ;
#14513 = DIRECTION ( 'NONE',  ( -1.000000000000000000, -0.000000000000000000, -0.000000000000000000 ) ) ;
#14514 = CARTESIAN_POINT ( 'NONE',  ( 7.000000000000000000, 0.000000000000000000, -12.00000000000000000 ) ) ;
#14515 = ORIENTED_EDGE ( 'NONE', *, *, #14325, .T. ) ;
#14516 = CARTESIAN_POINT ( 'NONE',  ( 16.56753206892534891, -0.009369540855502522109, 0.001549402974394259360 ) ) ;
#14517 = CARTESIAN_POINT ( 'NONE',  ( 2.353870697619111940, 10.00946331859664085, 8.216087327472971324 ) ) ;
#14518 = VECTOR ( 'NONE', #12681, 1000.000000000000000 ) ;
#14519 = DIRECTION ( 'NONE',  ( 0.000000000000000000, 0.000000000000000000, -1.000000000000000000 ) ) ;
#14520 = PRESENTATION_LAYER_ASSIGNMENT (  '', '', ( #6598 ) ) ;
#14521 = CARTESIAN_POINT ( 'NONE',  ( 16.56679352167444819, -0.006618561353600137254, -0.006526964904752322223 ) ) ;
#14522 = DIRECTION ( 'NONE',  ( 0.000000000000000000, 0.000000000000000000, 1.000000000000000000 ) ) ;
#14523 = EDGE_CURVE ( 'NONE', #11535, #9475, #17162, .T. ) ;
#14524 = CARTESIAN_POINT ( 'NONE',  ( 2.636624412714994037, -14.46769361191274328, -6.973567714907344950 ) ) ;
#14525 = ORIENTED_EDGE ( 'NONE', *, *, #10930, .F. ) ;
#14526 = CARTESIAN_POINT ( 'NONE',  ( 2.320520222537155064, -14.32454429810361951, -6.542539914240126819 ) ) ;
#14528 = EDGE_LOOP ( 'NONE', ( #15803, #8448, #6431, #8997 ) ) ;
#14527 = DIRECTION ( 'NONE',  ( 0.7635533937278216055, 0.6071939193889560604, 0.2197766120036526161 ) ) ;
#14529 = LINE ( 'NONE', #12907, #3609 ) ;
#14530 = EDGE_CURVE ( 'NONE', #13827, #2439, #18609, .T. ) ;
#14531 = VECTOR ( 'NONE', #10662, 1000.000000000000000 ) ;
#14532 = CARTESIAN_POINT ( 'NONE',  ( 0.000000000000000000, 0.000000000000000000, 0.000000000000000000 ) ) ;
#14533 = EDGE_LOOP ( 'NONE', ( #10497, #3277, #5591, #9968 ) ) ;
#14534 = CARTESIAN_POINT ( 'NONE',  ( 2.636624412715384391, -11.60464335004044223, -11.10302021258006278 ) ) ;
#14535 = CARTESIAN_POINT ( 'NONE',  ( 1.391479049022300574, -7.500000000000000888, -14.80352021213832536 ) ) ;
#14536 =( BOUNDED_SURFACE ( )  B_SPLINE_SURFACE ( 3, 1, ( 
 ( #6981, #6877 ),
 ( #15385, #9818 ),
 ( #12699, #6789 ),
 ( #18532, #14327 ) ),
 .UNSPECIFIED., .F., .F., .T. ) 
 B_SPLINE_SURFACE_WITH_KNOTS ( ( 4, 4 ),
 ( 2, 2 ),
 ( 0.000000000000000000, 1.000000000000000000 ),
 ( 0.000000000000000000, 1.000000000000000000 ),
 .UNSPECIFIED. ) 
 GEOMETRIC_REPRESENTATION_ITEM ( )  RATIONAL_B_SPLINE_SURFACE ( (
 ( 1.000000000000000000, 1.000000000000000000),
 ( 0.9933953342250438912, 0.8357391271907739227),
 ( 0.9933953342250438912, 0.8357391271907739227),
 ( 1.000000000000000000, 1.000000000000000000) ) ) 
 REPRESENTATION_ITEM ( '' )  SURFACE ( )  );
#14537 = ORIENTED_EDGE ( 'NONE', *, *, #14818, .T. ) ;
#14538 = LINE ( 'NONE', #8713, #3576 ) ;
#14539 = CARTESIAN_POINT ( 'NONE',  ( 2.636624412715137478, -2.862162146983530775, 15.80357026013314048 ) ) ;
#14540 = VECTOR ( 'NONE', #2308, 1000.000000000000000 ) ;
#14541 = CARTESIAN_POINT ( 'NONE',  ( 0.3150692679895994996, -4.391039771493759680, 13.01874238516608884 ) ) ;
#14542 = CARTESIAN_POINT ( 'NONE',  ( 2.636624412714134280, 2.862162146984768896, 15.80357026013147426 ) ) ;
#14543 = VECTOR ( 'NONE', #17071, 1000.000000000000000 ) ;
#14544 =( GEOMETRIC_REPRESENTATION_CONTEXT ( 3 ) GLOBAL_UNCERTAINTY_ASSIGNED_CONTEXT ( ( #5379 ) ) GLOBAL_UNIT_ASSIGNED_CONTEXT ( ( #992, #11326, #17330 ) ) REPRESENTATION_CONTEXT ( 'NONE', 'WORKASPACE' ) );
#14545 = AXIS2_PLACEMENT_3D ( 'NONE', #15146, #2060, #2234 ) ;
#14546 = CARTESIAN_POINT ( 'NONE',  ( 2.636624412714237309, 15.80357026013209953, 2.862162146984226663 ) ) ;
#14547 = CARTESIAN_POINT ( 'NONE',  ( 2.747332970342022840, 11.45495994260734918, -11.66639548242795144 ) ) ;
#14548 = EDGE_CURVE ( 'NONE', #9110, #3117, #6870, .T. ) ;
#14549 = DIRECTION ( 'NONE',  ( -1.000000000000000000, 0.000000000000000000, 0.000000000000000000 ) ) ;
#14550 = CARTESIAN_POINT ( 'NONE',  ( 1.846524061778020531, 3.506196582971103926, 11.93805390544202361 ) ) ;
#14551 = DIRECTION ( 'NONE',  ( -0.9034263296138843602, 0.000000000000000000, -0.4287433579198459133 ) ) ;
#14552 = VECTOR ( 'NONE', #4333, 1000.000000000000000 ) ;
#14553 = EDGE_LOOP ( 'NONE', ( #13682, #12737, #7264, #1785, #17274 ) ) ;
#14554 = FACE_OUTER_BOUND ( 'NONE', #9456, .T. ) ;
#14555 = CARTESIAN_POINT ( 'NONE',  ( 3.950837973638668288, 14.41405733518061716, 1.958075594453843493 ) ) ;
#14556 = ORIENTED_EDGE ( 'NONE', *, *, #680, .T. ) ;
#14557 = EDGE_CURVE ( 'NONE', #17234, #257, #9433, .T. ) ;
#14558 = AXIS2_PLACEMENT_3D ( 'NONE', #6362, #4541, #14852 ) ;
#14559 = ORIENTED_EDGE ( 'NONE', *, *, #18240, .T. ) ;
#14560 = CARTESIAN_POINT ( 'NONE',  ( 1.136782529653004747, -40.00000000000000000, 3.000000000000000000 ) ) ;
#14561 = VERTEX_POINT ( 'NONE', #2645 ) ;
#14562 = CARTESIAN_POINT ( 'NONE',  ( 1.845756295923355328, -3.386818134580144690, 11.97166802574125022 ) ) ;
#14563 = VERTEX_POINT ( 'NONE', #1217 ) ;
#14564 = CARTESIAN_POINT ( 'NONE',  ( 0.3095370825347233956, 4.681152801286161846, 12.91933430393609683 ) ) ;
#14565 = CARTESIAN_POINT ( 'NONE',  ( 0.4862570985993252548, 13.44146924561381162, 3.580942890621718888 ) ) ;
#14566 = CARTESIAN_POINT ( 'NONE',  ( 2.123976203522053297, -7.899625852120107261, -13.47898556379321633 ) ) ;
#14567 = DIRECTION ( 'NONE',  ( 0.000000000000000000, -0.000000000000000000, 1.000000000000000000 ) ) ;
#14568 = CARTESIAN_POINT ( 'NONE',  ( 2.636624412717099908, 11.60464335004051861, -11.10302021258208249 ) ) ;
#14569 = FACE_OUTER_BOUND ( 'NONE', #6929, .T. ) ;
#14570 = CARTESIAN_POINT ( 'NONE',  ( 1.846138399168762989, 10.30487220521570357, 6.971848976711047641 ) ) ;
#14571 = FACE_OUTER_BOUND ( 'NONE', #13500, .T. ) ;
#14572 = CARTESIAN_POINT ( 'NONE',  ( 0.3151928476913591903, 13.73922860838471749, -0.0002082997484259338093 ) ) ;
#14573 = ADVANCED_FACE ( 'NONE', ( #13066 ), #14288, .T. ) ;
#14574 = ORIENTED_EDGE ( 'NONE', *, *, #1380, .F. ) ;
#14575 = ORIENTED_EDGE ( 'NONE', *, *, #11594, .F. ) ;
#14576 = AXIS2_PLACEMENT_3D ( 'NONE', #18113, #542, #15330 ) ;
#14577 = EDGE_CURVE ( 'NONE', #13171, #1377, #11452, .T. ) ;
#14578 = ORIENTED_EDGE ( 'NONE', *, *, #1816, .T. ) ;
#14579 = ORIENTED_EDGE ( 'NONE', *, *, #7020, .F. ) ;
#14580 = ORIENTED_EDGE ( 'NONE', *, *, #3866, .T. ) ;
#14581 = DIRECTION ( 'NONE',  ( 0.000000000000000000, 0.000000000000000000, 1.000000000000000000 ) ) ;
#14582 = CARTESIAN_POINT ( 'NONE',  ( 0.3170788640506441158, 13.74111462631963576, -0.1533108587036642600 ) ) ;
#14583 = DIRECTION ( 'NONE',  ( 0.7561779333270775005, -0.03481510524965699543, 0.6534392409364816467 ) ) ;
#14584 = VERTEX_POINT ( 'NONE', #18895 ) ;
#14585 = DIRECTION ( 'NONE',  ( -1.000000000000000000, 1.387778780781445478E-15, 0.000000000000000000 ) ) ;
#14586 = CARTESIAN_POINT ( 'NONE',  ( 16.57210152137263393, -0.01402404281923042353, -0.003862718596009419997 ) ) ;
#14587 = B_SPLINE_CURVE_WITH_KNOTS ( 'NONE', 3,
 ( #6087, #11917, #3399, #4941, #10481, #13438 ),
 .UNSPECIFIED., .F., .F.,
 ( 4, 2, 4 ),
 ( 0.000000000000000000, 0.0001828790815886946713, 0.0003657581631773893427 ),
 .UNSPECIFIED. ) ;
#14588 = LINE ( 'NONE', #10486, #15849 ) ;
#14589 = CARTESIAN_POINT ( 'NONE',  ( 2.002547531651519996, 3.242439124566649511, 12.17374746633579541 ) ) ;
#14590 = DIRECTION ( 'NONE',  ( -1.000000000000000000, -0.000000000000000000, -0.000000000000000000 ) ) ;
#14591 = CARTESIAN_POINT ( 'NONE',  ( 2.636624412714236865, 0.000000000000000000, -16.06066017081991149 ) ) ;
#14592 = CARTESIAN_POINT ( 'NONE',  ( 0.4862570985993235340, -0.7479633556561480212, -13.89016912371018186 ) ) ;
#14593 = CARTESIAN_POINT ( 'NONE',  ( -194.9999999999999716, 4.999999999999973355, 3.000000000000000000 ) ) ;
#14594 = DIRECTION ( 'NONE',  ( -0.000000000000000000, 1.000000000000000000, 0.000000000000000000 ) ) ;
#14595 = EDGE_LOOP ( 'NONE', ( #17896, #13905, #9496, #4700 ) ) ;
#14596 = ORIENTED_EDGE ( 'NONE', *, *, #7743, .F. ) ;
#14597 = EDGE_CURVE ( 'NONE', #11580, #6611, #79, .T. ) ;
#14598 = ADVANCED_FACE ( 'NONE', ( #4573 ), #4375, .T. ) ;
#14599 = EDGE_CURVE ( 'NONE', #6138, #15079, #12179, .T. ) ;
#14600 = ORIENTED_EDGE ( 'NONE', *, *, #14408, .T. ) ;
#14601 = VERTEX_POINT ( 'NONE', #3015 ) ;
#14602 = CARTESIAN_POINT ( 'NONE',  ( 16.56822296793089322, -0.007741272030791128758, 0.006547366384936715959 ) ) ;
#14603 = EDGE_LOOP ( 'NONE', ( #7461, #1727, #2627, #7606 ) ) ;
#14604 = CARTESIAN_POINT ( 'NONE',  ( 3.950837973638675393, 2.591948120961804936, 14.31366178983254578 ) ) ;
#14605 = LINE ( 'NONE', #1523, #6861 ) ;
#14606 = CARTESIAN_POINT ( 'NONE',  ( 1.342453679581834924, 14.34050741580211508, -3.649820028552582585 ) ) ;
#14607 = B_SPLINE_CURVE_WITH_KNOTS ( 'NONE', 3,
 ( #5529, #2664, #2750, #1331, #8597, #17025, #2839, #11379, #6888, #2561, #12710, #18541, #11474 ),
 .UNSPECIFIED., .F., .F.,
 ( 4, 3, 3, 3, 4 ),
 ( 1.897353801849632760E-18, 0.0002299804304191482569, 0.0004599608082120252260, 0.0006467586077648016917, 0.0008336169836825988323 ),
 .UNSPECIFIED. ) ;
#14608 = DIRECTION ( 'NONE',  ( -1.000000000000000000, 0.000000000000000000, 0.000000000000000000 ) ) ;
#14609 = CIRCLE ( 'NONE', #11562, 5.000000000000004441 ) ;
#14610 = VERTEX_POINT ( 'NONE', #10496 ) ;
#14611 = DIRECTION ( 'NONE',  ( -1.000000000000000000, -0.000000000000000000, -0.000000000000000000 ) ) ;
#14612 = CARTESIAN_POINT ( 'NONE',  ( 0.3151930723728477157, -4.172946285306481151, -13.09040889075574476 ) ) ;
#14613 = CARTESIAN_POINT ( 'NONE',  ( 3.686287386450715076E-15, -16.60000000000000142, 25.01316734529526187 ) ) ;
#14614 = CARTESIAN_POINT ( 'NONE',  ( 1.847034903785822246, 11.76058231742745797, 4.063013886994747637 ) ) ;
#14615 = CARTESIAN_POINT ( 'NONE',  ( 1.846138399168762101, -6.971848976711082280, 10.30487220521567693 ) ) ;
#14616 = DIRECTION ( 'NONE',  ( 0.000000000000000000, 0.000000000000000000, -1.000000000000000000 ) ) ;
#14617 = VERTEX_POINT ( 'NONE', #16231 ) ;
#14618 = AXIS2_PLACEMENT_3D ( 'NONE', #14706, #8793, #17782 ) ;
#14619 = CARTESIAN_POINT ( 'NONE',  ( -6.000000000000000000, 20.00000000000000000, 3.000000000000000000 ) ) ;
#14620 = VECTOR ( 'NONE', #11677, 1000.000000000000000 ) ;
#14622 = ORIENTED_EDGE ( 'NONE', *, *, #4417, .T. ) ;
#14621 = CARTESIAN_POINT ( 'NONE',  ( 0.4862570985993252548, 5.003653737315486794, 12.97920246947881395 ) ) ;
#14623 = ADVANCED_FACE ( 'NONE', ( #3112 ), #16031, .T. ) ;
#14624 = CARTESIAN_POINT ( 'NONE',  ( 1.918918678667045574, 12.08296592096908384, 3.258447776119875350 ) ) ;
#14625 = ADVANCED_FACE ( 'NONE', ( #13546 ), #14788, .T. ) ;
#14626 = EDGE_CURVE ( 'NONE', #1746, #9296, #13359, .T. ) ;
#14627 = B_SPLINE_CURVE_WITH_KNOTS ( 'NONE', 3,
 ( #17456, #13150, #14487, #8567, #2904, #14772 ),
 .UNSPECIFIED., .F., .F.,
 ( 4, 2, 4 ),
 ( 5.421010862427522170E-19, 0.0001825746017570583442, 0.0003651492035141161462 ),
 .UNSPECIFIED. ) ;
#14628 = CARTESIAN_POINT ( 'NONE',  ( 0.000000000000000000, 0.000000000000000000, 10.00000000000000000 ) ) ;
#14629 = B_SPLINE_CURVE_WITH_KNOTS ( 'NONE', 3,
 ( #1650, #16661, #13502, #6536 ),
 .UNSPECIFIED., .F., .F.,
 ( 4, 4 ),
 ( 6.158879127553505933E-17, 0.002004993803842649181 ),
 .UNSPECIFIED. ) ;
#14630 = EDGE_CURVE ( 'NONE', #18099, #6002, #3499, .T. ) ;
#14631 = CIRCLE ( 'NONE', #899, 0.5000000000000004441 ) ;
#14632 = EDGE_LOOP ( 'NONE', ( #197, #3753, #7696 ) ) ;
#14633 = CARTESIAN_POINT ( 'NONE',  ( 3.950837973638675393, -13.10350451991845055, 6.316429227969417859 ) ) ;
#14634 = CARTESIAN_POINT ( 'NONE',  ( 2.611994420159011732, -7.500000000000000888, -15.68429332095010231 ) ) ;
#14635 = B_SPLINE_CURVE_WITH_KNOTS ( 'NONE', 3,
 ( #12024, #6190, #4571, #17468, #10394, #1409 ),
 .UNSPECIFIED., .F., .F.,
 ( 4, 2, 4 ),
 ( 8.940560153363745023E-19, 0.0001828790815886946442, 0.0003657581631773883669 ),
 .UNSPECIFIED. ) ;
#14636 = ORIENTED_EDGE ( 'NONE', *, *, #5521, .F. ) ;
#14637 = CARTESIAN_POINT ( 'NONE',  ( 0.8740779401508875779, -3.609949156401464965, 13.83508928787437142 ) ) ;
#14638 = CARTESIAN_POINT ( 'NONE',  ( 1.918921323896324083, 4.466082741316370175, -11.69058285425785648 ) ) ;
#14639 = FACE_OUTER_BOUND ( 'NONE', #3041, .T. ) ;
#14640 = SHAPE_REPRESENTATION_RELATIONSHIP ( 'NONE' , 'NONE' ,  #12894, #1240 ) ;
#14641 = CARTESIAN_POINT ( 'NONE',  ( 0.3170788640506440603, -7.952793437297492218, -11.20690911610912543 ) ) ;
#14642 = PLANE ( 'NONE',  #4522 ) ;
#14643 = DIRECTION ( 'NONE',  ( -1.000000000000000000, -0.000000000000000000, -0.000000000000000000 ) ) ;
#14644 = CARTESIAN_POINT ( 'NONE',  ( 18.75000000000000000, 0.000000000000000000, 0.000000000000000000 ) ) ;
#14645 = DIRECTION ( 'NONE',  ( -1.000000000000000000, -0.000000000000000000, -0.000000000000000000 ) ) ;
#14646 = ORIENTED_EDGE ( 'NONE', *, *, #2129, .T. ) ;
#14647 = CARTESIAN_POINT ( 'NONE',  ( 14.99999999999999289, 20.00000000000000000, 0.000000000000000000 ) ) ;
#14648 = CARTESIAN_POINT ( 'NONE',  ( 0.3170788640506440603, -13.11595226728160668, 4.100430649997911736 ) ) ;
#14649 = VERTEX_POINT ( 'NONE', #10201 ) ;
#14650 = ORIENTED_EDGE ( 'NONE', *, *, #13633, .T. ) ;
#14651 = DIRECTION ( 'NONE',  ( -0.000000000000000000, -0.000000000000000000, 1.000000000000000000 ) ) ;
#14652 = EDGE_CURVE ( 'NONE', #8892, #7279, #3737, .T. ) ;
#14653 = EDGE_LOOP ( 'NONE', ( #9160, #1273, #9250, #3612 ) ) ;
#14654 = CARTESIAN_POINT ( 'NONE',  ( 16.57778382496167424, -0.007244066302947598825, 0.01306626476309386518 ) ) ;
#14655 = ORIENTED_EDGE ( 'NONE', *, *, #7591, .T. ) ;
#14656 = CARTESIAN_POINT ( 'NONE',  ( 1.847461586945727152, 10.04711372545055781, -7.341074796295831817 ) ) ;
#14657 = CARTESIAN_POINT ( 'NONE',  ( 1.846138399168762101, -7.646096044339961040, 9.815003036200383946 ) ) ;
#14658 = LINE ( 'NONE', #17926, #7849 ) ;
#14659 = CARTESIAN_POINT ( 'NONE',  ( 0.3142011359265368120, 4.608101617236774139, 12.94258167753013922 ) ) ;
#14660 = B_SPLINE_CURVE_WITH_KNOTS ( 'NONE', 3,
 ( #12817, #14072, #977, #18644, #12626, #5543, #17212 ),
 .UNSPECIFIED., .F., .F.,
 ( 4, 3, 4 ),
 ( 3.198396408832238080E-18, 0.0002299780670421061460, 0.0004597478348665241538 ),
 .UNSPECIFIED. ) ;
#14661 = CARTESIAN_POINT ( 'NONE',  ( 0.3145734862173252822, -8.321353293018908914, 10.93207848441430130 ) ) ;
#14662 = CARTESIAN_POINT ( 'NONE',  ( 0.4862570985993235340, 11.67702470553376060, -7.559321496869298329 ) ) ;
#14663 = FILL_AREA_STYLE_COLOUR ( '', #10566 ) ;
#14664 = CARTESIAN_POINT ( 'NONE',  ( 2.636624412714756005, -2.161493821597335607, 15.91454522070219113 ) ) ;
#14665 = DIRECTION ( 'NONE',  ( 0.000000000000000000, -1.000000000000000000, 0.000000000000000000 ) ) ;
#14666 = EDGE_CURVE ( 'NONE', #3191, #10770, #5689, .T. ) ;
#14667 = CARTESIAN_POINT ( 'NONE',  ( 0.3142011359265305392, 13.73310835363014348, -0.3830873813806805472 ) ) ;
#14668 = PRODUCT_RELATED_PRODUCT_CATEGORY ( 'part', '', ( #684 ) ) ;
#14669 = DIRECTION ( 'NONE',  ( -0.000000000000000000, -0.000000000000000000, 1.000000000000000000 ) ) ;
#14670 = EDGE_CURVE ( 'NONE', #15279, #11185, #12714, .T. ) ;
#14671 = ORIENTED_EDGE ( 'NONE', *, *, #6837, .F. ) ;
#14672 = EDGE_CURVE ( 'NONE', #4027, #3394, #7402, .T. ) ;
#14673 = VERTEX_POINT ( 'NONE', #3608 ) ;
#14674 = EDGE_LOOP ( 'NONE', ( #30, #5479, #5023, #9514 ) ) ;
#14675 = VERTEX_POINT ( 'NONE', #12221 ) ;
#14676 = CARTESIAN_POINT ( 'NONE',  ( 2.002547531651519996, 4.532360870844327039, 11.75462648437103752 ) ) ;
#14677 = DIRECTION ( 'NONE',  ( 0.000000000000000000, 0.000000000000000000, 1.000000000000000000 ) ) ;
#14678 = DIRECTION ( 'NONE',  ( -0.000000000000000000, -0.5000000000000004441, 0.8660254037844383745 ) ) ;
#14679 = EDGE_LOOP ( 'NONE', ( #18007, #12031, #13728, #6299 ) ) ;
#14680 = LINE ( 'NONE', #17660, #3181 ) ;
#14681 = DIRECTION ( 'NONE',  ( -1.000000000000000000, -0.000000000000000000, -0.000000000000000000 ) ) ;
#14682 = AXIS2_PLACEMENT_3D ( 'NONE', #12872, #942, #5696 ) ;
#14683 = CARTESIAN_POINT ( 'NONE',  ( 0.000000000000000000, 0.000000000000000000, 11.00000000000000000 ) ) ;
#14684 = CARTESIAN_POINT ( 'NONE',  ( 0.4862570985993252548, -3.580942890621766406, 13.44146924561379741 ) ) ;
#14685 = DIRECTION ( 'NONE',  ( 0.000000000000000000, 0.000000000000000000, -1.000000000000000000 ) ) ;
#14686 = EDGE_CURVE ( 'NONE', #11651, #4800, #3697, .T. ) ;
#14687 = DIRECTION ( 'NONE',  ( 1.000000000000000000, 0.000000000000000000, 0.000000000000000000 ) ) ;
#14688 = CARTESIAN_POINT ( 'NONE',  ( 2.636624412715137478, -2.862162146983530775, 15.80357026013314048 ) ) ;
#14689 = CARTESIAN_POINT ( 'NONE',  ( 1.560000000000000053, 0.8660254037844389297, -1.500000000000000000 ) ) ;
#14690 = CARTESIAN_POINT ( 'NONE',  ( 0.3145734862173198421, -7.825584895511444650, -11.29227530924455003 ) ) ;
#14691 = ORIENTED_EDGE ( 'NONE', *, *, #7100, .F. ) ;
#14692 = EDGE_CURVE ( 'NONE', #11575, #14465, #13919, .T. ) ;
#14693 = ORIENTED_EDGE ( 'NONE', *, *, #14843, .T. ) ;
#14694 = VERTEX_POINT ( 'NONE', #12486 ) ;
#14695 = ORIENTED_EDGE ( 'NONE', *, *, #4413, .T. ) ;
#14696 = DIRECTION ( 'NONE',  ( 0.000000000000000000, 0.000000000000000000, 1.000000000000000000 ) ) ;
#14697 = VERTEX_POINT ( 'NONE', #2179 ) ;
#14698 = CARTESIAN_POINT ( 'NONE',  ( 2.750000000000000000, 0.000000000000000000, 0.000000000000000000 ) ) ;
#14699 = PLANE ( 'NONE',  #3187 ) ;
#14700 = FACE_OUTER_BOUND ( 'NONE', #8030, .T. ) ;
#14701 = AXIS2_PLACEMENT_3D ( 'NONE', #18096, #972, #702 ) ;
#14702 = CARTESIAN_POINT ( 'NONE',  ( 16.56872352241294521, -0.001442253899401298341, 0.01033355228142499027 ) ) ;
#14703 = ORIENTED_EDGE ( 'NONE', *, *, #8490, .F. ) ;
#14704 = CARTESIAN_POINT ( 'NONE',  ( -0.7623231285407784386, 7.500000000000000000, -14.39641017501654829 ) ) ;
#14705 = CARTESIAN_POINT ( 'NONE',  ( -194.9999999999999716, -5.000000000000024869, 11.00000000000000000 ) ) ;
#14706 = CARTESIAN_POINT ( 'NONE',  ( 0.000000000000000000, 0.000000000000000000, 0.000000000000000000 ) ) ;
#14707 = B_SPLINE_CURVE_WITH_KNOTS ( 'NONE', 3,
 ( #1707, #10610, #3025, #7555, #13368, #283 ),
 .UNSPECIFIED., .F., .F.,
 ( 4, 2, 4 ),
 ( 2.468197616305571356E-18, 0.0002017457492448094245, 0.0004034914984896164096 ),
 .UNSPECIFIED. ) ;
#14708 = CARTESIAN_POINT ( 'NONE',  ( 8.438534575730034959, 6.598402093327880635, 1.899950616255211111 ) ) ;
#14709 = ADVANCED_FACE ( 'NONE', ( #4860 ), #12371, .F. ) ;
#14710 = CARTESIAN_POINT ( 'NONE',  ( 0.3151930723728440520, 13.04315954105015152, 4.318364831037635021 ) ) ;
#14711 = CARTESIAN_POINT ( 'NONE',  ( 0.3170788640506440603, 4.392045232375992647, -13.02120094575823472 ) ) ;
#14712 = ORIENTED_EDGE ( 'NONE', *, *, #6680, .T. ) ;
#14713 = AXIS2_PLACEMENT_3D ( 'NONE', #4432, #13217, #2318 ) ;
#14714 = B_SPLINE_CURVE_WITH_KNOTS ( 'NONE', 3,
 ( #3689, #13644, #14972, #5030 ),
 .UNSPECIFIED., .F., .F.,
 ( 4, 4 ),
 ( 3.019714627835872489E-16, 0.002004993803842318283 ),
 .UNSPECIFIED. ) ;
#14715 = CARTESIAN_POINT ( 'NONE',  ( 2.705023505549862595, -10.24007717649586624, 8.489131503859741912 ) ) ;
#14717 = VERTEX_POINT ( 'NONE', #15351 ) ;
#14716 = CARTESIAN_POINT ( 'NONE',  ( 1.977228804421669262, 6.152949558600965041, 14.12033626431027322 ) ) ;
#14718 = LINE ( 'NONE', #11579, #1134 ) ;
#14719 = CARTESIAN_POINT ( 'NONE',  ( 16.56753206892534891, -0.004253784598196239108, 0.008490833999798910042 ) ) ;
#14720 = ORIENTED_EDGE ( 'NONE', *, *, #14670, .T. ) ;
#14721 = CARTESIAN_POINT ( 'NONE',  ( 3.377929128793395908, -7.136734442940921852, 12.02809354424098665 ) ) ;
#14722 = UNCERTAINTY_MEASURE_WITH_UNIT (LENGTH_MEASURE( 1.000000000000000082E-05 ), #10856, 'distance_accuracy_value', 'NONE');
#14723 = CARTESIAN_POINT ( 'NONE',  ( 6.154177238273381256, -7.500000000000001776, -12.51861270110025792 ) ) ;
#14724 = VERTEX_POINT ( 'NONE', #3511 ) ;
#14725 = CARTESIAN_POINT ( 'NONE',  ( 0.3095370825347224519, -3.806662003783507497, 13.20347358821913275 ) ) ;
#14726 = LINE ( 'NONE', #11778, #1508 ) ;
#14727 = PLANE ( 'NONE',  #6582 ) ;
#14728 = EDGE_CURVE ( 'NONE', #13924, #14584, #17656, .T. ) ;
#14729 = EDGE_CURVE ( 'NONE', #911, #18408, #11068, .T. ) ;
#14730 = ADVANCED_FACE ( 'NONE', ( #9248 ), #14319, .F. ) ;
#14731 = ORIENTED_EDGE ( 'NONE', *, *, #332, .F. ) ;
#14732 = AXIS2_PLACEMENT_3D ( 'NONE', #46, #13328, #245 ) ;
#14733 = FACE_OUTER_BOUND ( 'NONE', #525, .T. ) ;
#14734 = CARTESIAN_POINT ( 'NONE',  ( 3.950837973638675393, 6.888253895133292559, 12.81214529934977797 ) ) ;
#14735 = CARTESIAN_POINT ( 'NONE',  ( 0.3720661004400040439, -13.34435358167250207, -3.575426119359325750 ) ) ;
#14736 = CARTESIAN_POINT ( 'NONE',  ( 3.950837973638668288, 14.41405733518061716, 1.958075594453843493 ) ) ;
#14737 = DIRECTION ( 'NONE',  ( 1.000000000000000000, -2.891205793294679312E-16, 0.000000000000000000 ) ) ;
#14738 = ORIENTED_EDGE ( 'NONE', *, *, #6910, .F. ) ;
#14739 = CARTESIAN_POINT ( 'NONE',  ( 0.3142011359265323156, -7.762194356530850214, 11.33549115679420538 ) ) ;
#14740 = CARTESIAN_POINT ( 'NONE',  ( 16.56753206892534891, 0.009369540855502130061, 0.001549402974393180796 ) ) ;
#14741 = ORIENTED_EDGE ( 'NONE', *, *, #9263, .T. ) ;
#14742 = VERTEX_POINT ( 'NONE', #742 ) ;
#14743 = DIRECTION ( 'NONE',  ( -1.000000000000000000, 0.000000000000000000, 0.000000000000000000 ) ) ;
#14744 = AXIS2_PLACEMENT_3D ( 'NONE', #14560, #10069, #11693 ) ;
#14745 = ORIENTED_EDGE ( 'NONE', *, *, #71, .T. ) ;
#14746 = DIRECTION ( 'NONE',  ( -1.000000000000000000, -0.000000000000000000, -0.000000000000000000 ) ) ;
#14747 = VERTEX_POINT ( 'NONE', #10786 ) ;
#14748 = B_SPLINE_CURVE_WITH_KNOTS ( 'NONE', 3,
 ( #11472, #14517, #7076, #10321, #96, #8792 ),
 .UNSPECIFIED., .F., .F.,
 ( 4, 2, 4 ),
 ( 8.673617379884035472E-19, 0.001500839035891548753, 0.003001678071783096639 ),
 .UNSPECIFIED. ) ;
#14749 = AXIS2_PLACEMENT_3D ( 'NONE', #13473, #14811, #6576 ) ;
#14750 = VECTOR ( 'NONE', #3301, 999.9999999999998863 ) ;
#14751 = CARTESIAN_POINT ( 'NONE',  ( 3.074695600507405757, 7.366518011945858646, 13.70113613813188458 ) ) ;
#14752 = CARTESIAN_POINT ( 'NONE',  ( 2.747332970342022840, 2.705255688518072965, -16.12459247543623064 ) ) ;
#14753 = CARTESIAN_POINT ( 'NONE',  ( 1.918921323896325193, -4.466082741316288462, 11.69058285425789201 ) ) ;
#14754 = UNCERTAINTY_MEASURE_WITH_UNIT (LENGTH_MEASURE( 1.000000000000000082E-05 ), #15885, 'distance_accuracy_value', 'NONE');
#14755 = CARTESIAN_POINT ( 'NONE',  ( 8.438534575730034959, 4.221456476902743837, -5.415535776177475391 ) ) ;
#14756 = CYLINDRICAL_SURFACE ( 'NONE', #18784, 2.500000000000000000 ) ;
#14757 = PLANE ( 'NONE',  #13527 ) ;
#14758 = LINE ( 'NONE', #148, #4833 ) ;
#14759 = EDGE_CURVE ( 'NONE', #102, #18437, #18512, .T. ) ;
#14760 = CARTESIAN_POINT ( 'NONE',  ( 16.56753206892534891, 0.004253784598196178393, -0.008490833999798937798 ) ) ;
#14761 = LINE ( 'NONE', #4450, #3569 ) ;
#14762 = AXIS2_PLACEMENT_3D ( 'NONE', #13443, #6384, #17850 ) ;
#14763 = STYLED_ITEM ( 'NONE', ( #17292 ), #10342 ) ;
#14764 = CARTESIAN_POINT ( 'NONE',  ( 1.846613052777650976, -11.72395935470501627, 4.166957398589803852 ) ) ;
#14765 = DIRECTION ( 'NONE',  ( -1.000000000000000000, -0.000000000000000000, -0.000000000000000000 ) ) ;
#14766 = EDGE_LOOP ( 'NONE', ( #8445, #1275, #2786, #9157 ) ) ;
#14767 = EDGE_CURVE ( 'NONE', #7666, #12252, #12395, .T. ) ;
#14768 = EDGE_LOOP ( 'NONE', ( #15153, #15291, #3217, #17695, #3527, #8385, #7880, #3462 ) ) ;
#14769 = VERTEX_POINT ( 'NONE', #16797 ) ;
#14770 = VERTEX_POINT ( 'NONE', #12670 ) ;
#14771 = CARTESIAN_POINT ( 'NONE',  ( 0.3142014840576502488, -7.762239086932773091, -11.33546131209471142 ) ) ;
#14772 = CARTESIAN_POINT ( 'NONE',  ( 1.846138399168762101, -0.4167076046094680408, -12.43476674860266940 ) ) ;
#14773 = CARTESIAN_POINT ( 'NONE',  ( 1.846138399168762101, -7.646096044339819819, -9.815003036200495856 ) ) ;
#14774 = VERTEX_POINT ( 'NONE', #5671 ) ;
#14775 = LINE ( 'NONE', #3305, #7482 ) ;
#14776 = DIRECTION ( 'NONE',  ( -1.000000000000000000, -0.000000000000000000, -0.000000000000000000 ) ) ;
#14777 = CIRCLE ( 'NONE', #10824, 16.06066017081991149 ) ;
#14778 = CARTESIAN_POINT ( 'NONE',  ( 2.636624412716045196, 11.10302021257998994, -11.60464335004042447 ) ) ;
#14779 = CARTESIAN_POINT ( 'NONE',  ( 0.3058872367615230181, -4.821066432589238282, -12.87003593440633331 ) ) ;
#14780 = CARTESIAN_POINT ( 'NONE',  ( 1.977228804422749064, -1.488378900182820264, -15.33060379559159259 ) ) ;
#14781 = ADVANCED_FACE ( 'NONE', ( #9713 ), #16280, .F. ) ;
#14782 = CARTESIAN_POINT ( 'NONE',  ( 1.846822687350019754, 11.92063725419904152, -3.566003975885565946 ) ) ;
#14783 = DIRECTION ( 'NONE',  ( -0.000000000000000000, -0.000000000000000000, -1.000000000000000000 ) ) ;
#14784 = EDGE_CURVE ( 'NONE', #819, #13856, #15820, .T. ) ;
#14785 = CARTESIAN_POINT ( 'NONE',  ( 3.950837973638668288, 0.000000000000000000, 0.000000000000000000 ) ) ;
#14786 = EDGE_CURVE ( 'NONE', #13455, #15874, #2347, .T. ) ;
#14787 = B_SPLINE_CURVE_WITH_KNOTS ( 'NONE', 3,
 ( #11021, #610, #3654, #2039, #16749, #1946 ),
 .UNSPECIFIED., .F., .F.,
 ( 4, 2, 4 ),
 ( 4.253224384355279651E-17, 0.0002014099069817287574, 0.0004028198139634150141 ),
 .UNSPECIFIED. ) ;
#14788 = CYLINDRICAL_SURFACE ( 'NONE', #13332, 5.000000000000000888 ) ;
#14789 = ORIENTED_EDGE ( 'NONE', *, *, #6704, .T. ) ;
#14790 = EDGE_LOOP ( 'NONE', ( #7451, #5731, #1517, #13071 ) ) ;
#14791 = CIRCLE ( 'NONE', #7175, 4.750000000000000000 ) ;
#14792 = ORIENTED_EDGE ( 'NONE', *, *, #2510, .T. ) ;
#14793 = ORIENTED_EDGE ( 'NONE', *, *, #10826, .F. ) ;
#14794 = VECTOR ( 'NONE', #11294, 1000.000000000000000 ) ;
#14795 = CARTESIAN_POINT ( 'NONE',  ( 3.512766787570769100, 13.55823433651956833, -6.535475144496838418 ) ) ;
#14796 = CIRCLE ( 'NONE', #15108, 1.500000000000000000 ) ;
#14797 = EDGE_CURVE ( 'NONE', #11439, #16313, #12574, .T. ) ;
#14798 = ORIENTED_EDGE ( 'NONE', *, *, #3580, .F. ) ;
#14799 = CARTESIAN_POINT ( 'NONE',  ( 1.861628059977344263, -6.879051339207215676, -10.38573835516720401 ) ) ;
#14800 = CARTESIAN_POINT ( 'NONE',  ( 0.4862570985993235340, -11.67702470553370553, 7.559321496869385371 ) ) ;
#14801 = CARTESIAN_POINT ( 'NONE',  ( 2.636624412716062071, -11.10302021258080352, -11.60464335004061454 ) ) ;
#14802 = FACE_OUTER_BOUND ( 'NONE', #12752, .T. ) ;
#14803 = ORIENTED_EDGE ( 'NONE', *, *, #2609, .T. ) ;
#14804 = CARTESIAN_POINT ( 'NONE',  ( 1.847034903785829574, -4.063013886994788493, 11.76058231742743665 ) ) ;
#14805 = CARTESIAN_POINT ( 'NONE',  ( -2.750000000000000000, 3.367778697655221012E-16, 10.00000000000000000 ) ) ;
#14806 = CARTESIAN_POINT ( 'NONE',  ( -6.454593536054757941, 2.712332671582286192, -12.00000000018538415 ) ) ;
#14807 = CARTESIAN_POINT ( 'NONE',  ( 16.56822296793089322, -0.009385634690641594599, -0.003834730849370937035 ) ) ;
#14808 = DIRECTION ( 'NONE',  ( -0.7635533937278214944, 0.6204116510013479857, 0.1790966170213943998 ) ) ;
#14809 = CIRCLE ( 'NONE', #13895, 16.06066017081991149 ) ;
#14810 = CIRCLE ( 'NONE', #8117, 5.000000000000000000 ) ;
#14811 = DIRECTION ( 'NONE',  ( 0.000000000000000000, 1.000000000000000000, -0.000000000000000000 ) ) ;
#14812 = EDGE_LOOP ( 'NONE', ( #579, #13340, #16008, #5065, #2584 ) ) ;
#14813 = CARTESIAN_POINT ( 'NONE',  ( 1.846822687350019754, 7.547953575784267066, -9.891732594446496662 ) ) ;
#14815 = VERTEX_POINT ( 'NONE', #9986 ) ;
#14814 = CARTESIAN_POINT ( 'NONE',  ( 3.377929128793393687, 12.02809354424100619, 7.136734442940879219 ) ) ;
#14816 = DIRECTION ( 'NONE',  ( -0.9034263296138843602, 0.000000000000000000, -0.4287433579198459133 ) ) ;
#14817 = ORIENTED_EDGE ( 'NONE', *, *, #8212, .F. ) ;
#14818 = EDGE_CURVE ( 'NONE', #13997, #8831, #15172, .T. ) ;
#14819 = CARTESIAN_POINT ( 'NONE',  ( 0.3095370825347233956, 13.73357284481724783, -0.4597470195090692657 ) ) ;
#14820 =( BOUNDED_SURFACE ( )  B_SPLINE_SURFACE ( 3, 1, ( 
 ( #18752, #3864 ),
 ( #8179, #14085 ),
 ( #11507, #15517 ),
 ( #15426, #14174 ) ),
 .UNSPECIFIED., .F., .F., .T. ) 
 B_SPLINE_SURFACE_WITH_KNOTS ( ( 4, 4 ),
 ( 2, 2 ),
 ( 0.000000000000000000, 1.000000000000000000 ),
 ( 0.000000000000000000, 1.000000000000000000 ),
 .UNSPECIFIED. ) 
 GEOMETRIC_REPRESENTATION_ITEM ( )  RATIONAL_B_SPLINE_SURFACE ( (
 ( 1.000000000000000000, 1.000000000000000000),
 ( 0.9593108457356467333, 0.9995965569486454649),
 ( 0.9593108457356467333, 0.9995965569486454649),
 ( 1.000000000000000000, 1.000000000000000000) ) ) 
 REPRESENTATION_ITEM ( '' )  SURFACE ( )  );
#14821 = EDGE_CURVE ( 'NONE', #4379, #9019, #6848, .T. ) ;
#14822 = ORIENTED_EDGE ( 'NONE', *, *, #5747, .T. ) ;
#14823 = FACE_OUTER_BOUND ( 'NONE', #13730, .T. ) ;
#14824 = CARTESIAN_POINT ( 'NONE',  ( 6.238556470687417921, -7.500000000000000888, -16.99999999974153297 ) ) ;
#14825 =( GEOMETRIC_REPRESENTATION_CONTEXT ( 3 ) GLOBAL_UNCERTAINTY_ASSIGNED_CONTEXT ( ( #3049 ) ) GLOBAL_UNIT_ASSIGNED_CONTEXT ( ( #15530, #8282, #2709 ) ) REPRESENTATION_CONTEXT ( 'NONE', 'WORKASPACE' ) );
#14826 = ORIENTED_EDGE ( 'NONE', *, *, #5587, .T. ) ;
#14827 = CARTESIAN_POINT ( 'NONE',  ( 16.56753206892534891, -0.009369540855502119653, -0.001549402974393242162 ) ) ;
#14828 = CARTESIAN_POINT ( 'NONE',  ( 0.000000000000000000, 0.000000000000000000, 2.500000000000000000 ) ) ;
#14829 = CARTESIAN_POINT ( 'NONE',  ( 1.861628059977342708, 11.66985327793199190, 4.358833901513087916 ) ) ;
#14830 = CARTESIAN_POINT ( 'NONE',  ( 0.4384471787762824757, -13.84291427302852107, 0.7363690479465839767 ) ) ;
#14831 = ORIENTED_EDGE ( 'NONE', *, *, #3955, .T. ) ;
#14832 = CARTESIAN_POINT ( 'NONE',  ( 1.847247051441591514, -10.16425585218606109, 7.177495230324669961 ) ) ;
#14833 = CARTESIAN_POINT ( 'NONE',  ( 2.949999999999999734, 0.000000000000000000, 0.000000000000000000 ) ) ;
#14834 = AXIS2_PLACEMENT_3D ( 'NONE', #17357, #7341, #13056 ) ;
#14835 = PRESENTATION_LAYER_ASSIGNMENT (  '', '', ( #15448 ) ) ;
#14836 = CARTESIAN_POINT ( 'NONE',  ( 1.342453679581834924, -14.34050741580204402, -3.649820028552883233 ) ) ;
#14837 = CARTESIAN_POINT ( 'NONE',  ( 3.664313757352978485, 12.42002390572636372, -7.012524439851359759 ) ) ;
#14838 = DIRECTION ( 'NONE',  ( 0.000000000000000000, 0.000000000000000000, 1.000000000000000000 ) ) ;
#14839 = VERTEX_POINT ( 'NONE', #5409 ) ;
#14840 = CARTESIAN_POINT ( 'NONE',  ( 1.846138399168762101, 7.646096044339892650, 9.815003036200437236 ) ) ;
#14841 = CARTESIAN_POINT ( 'NONE',  ( 3.950837973638676281, 14.31366178983253512, 2.591948120961855118 ) ) ;
#14842 = ORIENTED_EDGE ( 'NONE', *, *, #5440, .F. ) ;
#14843 = EDGE_CURVE ( 'NONE', #13257, #11387, #11342, .T. ) ;
#14844 = ADVANCED_FACE ( 'NONE', ( #2716 ), #6930, .T. ) ;
#14845 = ADVANCED_FACE ( 'NONE', ( #3975 ), #12967, .F. ) ;
#14846 = VERTEX_POINT ( 'NONE', #2522 ) ;
#14847 = CARTESIAN_POINT ( 'NONE',  ( -110.4113270445337918, -81.60345299795268659, -91.28051051278382033 ) ) ;
#14848 = ORIENTED_EDGE ( 'NONE', *, *, #16253, .F. ) ;
#14849 = CARTESIAN_POINT ( 'NONE',  ( 22.75000000000000000, 0.000000000000000000, 0.000000000000000000 ) ) ;
#14850 = ORIENTED_EDGE ( 'NONE', *, *, #3648, .T. ) ;
#14851 = CIRCLE ( 'NONE', #12413, 5.000000000000000888 ) ;
#14852 = DIRECTION ( 'NONE',  ( 0.000000000000000000, 0.000000000000000000, 1.000000000000000000 ) ) ;
#14853 = CARTESIAN_POINT ( 'NONE',  ( 15.00000000000000711, -45.00000000000000000, 6.000000000000000000 ) ) ;
#14854 = DIRECTION ( 'NONE',  ( 0.000000000000000000, -0.000000000000000000, 1.000000000000000000 ) ) ;
#14855 = AXIS2_PLACEMENT_3D ( 'NONE', #535, #895, #10754 ) ;
#14856 = PRODUCT_DEFINITION_SHAPE ( 'NONE', 'NONE',  #15021 ) ;
#14857 = CARTESIAN_POINT ( 'NONE',  ( 16.56782317627811096, -0.009439921864426449247, -0.002708056627497712563 ) ) ;
#14858 = SHAPE_REPRESENTATION ( 'spacer', ( #2030 ), #2329 ) ;
#14859 = FACE_OUTER_BOUND ( 'NONE', #7155, .T. ) ;
#14860 = CARTESIAN_POINT ( 'NONE',  ( 0.000000000000000000, 0.000000000000000000, 0.000000000000000000 ) ) ;
#14861 = CIRCLE ( 'NONE', #6636, 5.000000000000000000 ) ;
#14862 = APPLICATION_CONTEXT ( 'automotive_design' ) ;
#14863 = EDGE_CURVE ( 'NONE', #18437, #102, #1439, .T. ) ;
#14864 = CARTESIAN_POINT ( 'NONE',  ( 2.636624412714236865, 0.000000000000000000, 0.000000000000000000 ) ) ;
#14865 = VECTOR ( 'NONE', #10694, 1000.000000000000000 ) ;
#14866 = CARTESIAN_POINT ( 'NONE',  ( 3.074695600507349358, 10.75417554975707368, -11.23985886659415279 ) ) ;
#14867 =( GEOMETRIC_REPRESENTATION_CONTEXT ( 3 ) GLOBAL_UNCERTAINTY_ASSIGNED_CONTEXT ( ( #17044 ) ) GLOBAL_UNIT_ASSIGNED_CONTEXT ( ( #2448, #12682, #17168 ) ) REPRESENTATION_CONTEXT ( 'NONE', 'WORKASPACE' ) );
#14868 = CLOSED_SHELL ( 'NONE', ( #7426, #1422, #13809, #5207, #9525, #10602, #7421, #17437 ) ) ;
#14869 = CARTESIAN_POINT ( 'NONE',  ( 0.3095370825347234511, 11.38092634279639803, -7.700448427571746635 ) ) ;
#14870 = EDGE_LOOP ( 'NONE', ( #4746, #16707, #17724, #4719 ) ) ;
#14871 = ORIENTED_EDGE ( 'NONE', *, *, #7923, .T. ) ;
#14872 = EDGE_LOOP ( 'NONE', ( #14731, #13582, #17334, #18884 ) ) ;
#14873 = ORIENTED_EDGE ( 'NONE', *, *, #15665, .T. ) ;
#14874 = EDGE_CURVE ( 'NONE', #5775, #15079, #2436, .T. ) ;
#14875 = CARTESIAN_POINT ( 'NONE',  ( 0.3145729642390401870, 0.3065092323351212289, 13.73540280162740501 ) ) ;
#14876 = EDGE_CURVE ( 'NONE', #9110, #16337, #5544, .T. ) ;
#14877 = CARTESIAN_POINT ( 'NONE',  ( 0.3058872367615230181, 10.75034008168928068, -8.562166468153600718 ) ) ;
#14878 = B_SPLINE_CURVE_WITH_KNOTS ( 'NONE', 3,
 ( #7569, #17487, #3336, #16052, #13379, #17882 ),
 .UNSPECIFIED., .F., .F.,
 ( 4, 2, 4 ),
 ( 0.000000000000000000, 0.001500839035891551139, 0.003001678071783102277 ),
 .UNSPECIFIED. ) ;
#14879 = CARTESIAN_POINT ( 'NONE',  ( 2.002547531651519996, -7.942910686618100513, -9.778737580845787036 ) ) ;
#14880 = LINE ( 'NONE', #6287, #1640 ) ;
#14881 = DIRECTION ( 'NONE',  ( -0.000000000000000000, 1.000000000000000000, -0.000000000000000000 ) ) ;
#14882 = CARTESIAN_POINT ( 'NONE',  ( 0.4754618798421162973, 13.45049478164064638, -3.583352865732528425 ) ) ;
#14883 = CARTESIAN_POINT ( 'NONE',  ( 1.847380140988738262, 12.44273713935591097, -0.1101766933249076624 ) ) ;
#14884 = CARTESIAN_POINT ( 'NONE',  ( 1.562796894703937678, 0.000000000000000000, 0.000000000000000000 ) ) ;
#14885 = CARTESIAN_POINT ( 'NONE',  ( 1.254255976357671942, -5.487601330835209623, 13.61551404021223455 ) ) ;
#14886 = FACE_OUTER_BOUND ( 'NONE', #2608, .T. ) ;
#14887 = CARTESIAN_POINT ( 'NONE',  ( 1.104287921197080512E-14, -4.263167318348349610, 25.01316734529528674 ) ) ;
#14888 = CARTESIAN_POINT ( 'NONE',  ( 0.3151930723728413319, -8.013866567350813597, -11.16020735774775829 ) ) ;
#14889 = AXIS2_PLACEMENT_3D ( 'NONE', #10693, #13651, #12220 ) ;
#14890 = VERTEX_POINT ( 'NONE', #1199 ) ;
#14891 = ADVANCED_BREP_SHAPE_REPRESENTATION ( '', ( #16760, #2030 ), #809 ) ;
#14892 = ORIENTED_EDGE ( 'NONE', *, *, #9429, .F. ) ;
#14893 = VERTEX_POINT ( 'NONE', #9888 ) ;
#14894 = ORIENTED_EDGE ( 'NONE', *, *, #5927, .T. ) ;
#14895 = DIRECTION ( 'NONE',  ( -0.7561779333270775005, -0.5081796452863273084, 0.4122479608995688327 ) ) ;
#14896 = FACE_OUTER_BOUND ( 'NONE', #4918, .T. ) ;
#14897 = EDGE_CURVE ( 'NONE', #18099, #4894, #15720, .T. ) ;
#14898 = CARTESIAN_POINT ( 'NONE',  ( 2.002547531651519996, -9.778737580845755062, 7.942910686618138705 ) ) ;
#14899 = CARTESIAN_POINT ( 'NONE',  ( 3.353306896162456585, 10.44017738170056298, 9.252610477110303933 ) ) ;
#14900 = CARTESIAN_POINT ( 'NONE',  ( 1.977228804421969688, 1.488378900182327991, 15.33060379559086073 ) ) ;
#14901 = ORIENTED_EDGE ( 'NONE', *, *, #8046, .F. ) ;
#14902 = CARTESIAN_POINT ( 'NONE',  ( 3.605312816022526512, 7.499999999999999112, -16.26975837274198966 ) ) ;
#14903 = CIRCLE ( 'NONE', #16737, 14.54644660717763927 ) ;
#14904 = CARTESIAN_POINT ( 'NONE',  ( -66.35602477868049220, -10.00000000000000888, 5.999999999999999112 ) ) ;
#14905 = DIRECTION ( 'NONE',  ( 0.000000000000000000, 0.000000000000000000, 1.000000000000000000 ) ) ;
#14906 = DIRECTION ( 'NONE',  ( 1.000000000000000000, 0.000000000000000000, 0.000000000000000000 ) ) ;
#14907 = FILL_AREA_STYLE_COLOUR ( '', #7102 ) ;
#14908 = CARTESIAN_POINT ( 'NONE',  ( 0.3170788640506441158, -4.392045232375722641, -13.02120094575832709 ) ) ;
#14909 = ORIENTED_EDGE ( 'NONE', *, *, #3930, .F. ) ;
#14910 = EDGE_CURVE ( 'NONE', #998, #5396, #6171, .T. ) ;
#14911 = CARTESIAN_POINT ( 'NONE',  ( 2.949999999999999734, 3.306546357697853733E-16, -2.700000000000000178 ) ) ;
#14913 = VERTEX_POINT ( 'NONE', #7229 ) ;
#14912 = CARTESIAN_POINT ( 'NONE',  ( 0.3137051932979775248, 0.4596302728639756197, 13.73004976592202198 ) ) ;
#14914 = DIRECTION ( 'NONE',  ( -1.000000000000000000, -0.000000000000000000, 0.000000000000000000 ) ) ;
#14915 = CARTESIAN_POINT ( 'NONE',  ( -30.00000000000000355, -12.50000000000000178, 0.000000000000000000 ) ) ;
#14916 = B_SPLINE_CURVE_WITH_KNOTS ( 'NONE', 3,
 ( #16510, #15063, #17041, #5279, #18558, #6730 ),
 .UNSPECIFIED., .F., .F.,
 ( 4, 2, 4 ),
 ( 4.083989690778167730E-17, 0.0002014099069817300042, 0.0004028198139634191341 ),
 .UNSPECIFIED. ) ;
#14917 = ORIENTED_EDGE ( 'NONE', *, *, #13337, .F. ) ;
#14918 = CARTESIAN_POINT ( 'NONE',  ( 20.00000000000000711, -39.99999999999999289, 3.000000000000000000 ) ) ;
#14919 = CARTESIAN_POINT ( 'NONE',  ( 5.935721797378563203, -7.500000000000000888, -16.97606798286663476 ) ) ;
#14920 = ORIENTED_EDGE ( 'NONE', *, *, #6998, .F. ) ;
#14921 = DIRECTION ( 'NONE',  ( -0.7635533937278214944, -0.1790966170213966202, 0.6204116510013472086 ) ) ;
#14922 = DIRECTION ( 'NONE',  ( 0.000000000000000000, 0.000000000000000000, 1.000000000000000000 ) ) ;
#14923 = CARTESIAN_POINT ( 'NONE',  ( 16.56679352167444819, -0.008311568981098013675, -0.004162264567718770153 ) ) ;
#14924 = CARTESIAN_POINT ( 'NONE',  ( 8.522092701127531811, -1.786985377231985694, -6.722964936702116034 ) ) ;
#14925 = EDGE_CURVE ( 'NONE', #6426, #15645, #3035, .T. ) ;
#14926 = ORIENTED_EDGE ( 'NONE', *, *, #6631, .F. ) ;
#14927 = AXIS2_PLACEMENT_3D ( 'NONE', #6522, #18268, #5169 ) ;
#14928 = FILL_AREA_STYLE ('',( #2133 ) ) ;
#14929 = CARTESIAN_POINT ( 'NONE',  ( 2.002547531651519996, 12.57989064830759496, 0.6781519942172178350 ) ) ;
#14930 = CARTESIAN_POINT ( 'NONE',  ( 0.3145734862173260038, 10.93207848441433683, 8.321353293018871611 ) ) ;
#14931 =( BOUNDED_SURFACE ( )  B_SPLINE_SURFACE ( 3, 1, ( 
 ( #13209, #7492 ),
 ( #3164, #10157 ),
 ( #15981, #5942 ),
 ( #11787, #4528 ) ),
 .UNSPECIFIED., .F., .F., .T. ) 
 B_SPLINE_SURFACE_WITH_KNOTS ( ( 4, 4 ),
 ( 2, 2 ),
 ( 0.000000000000000000, 1.000000000000000000 ),
 ( 0.000000000000000000, 1.000000000000000000 ),
 .UNSPECIFIED. ) 
 GEOMETRIC_REPRESENTATION_ITEM ( )  RATIONAL_B_SPLINE_SURFACE ( (
 ( 1.000000000000000000, 1.000000000000000000),
 ( 0.7792777138730160313, 0.9689936506012927220),
 ( 0.7792777138730160313, 0.9689936506012927220),
 ( 1.000000000000000000, 1.000000000000000000) ) ) 
 REPRESENTATION_ITEM ( '' )  SURFACE ( )  );
#14932 = CARTESIAN_POINT ( 'NONE',  ( 2.179449471770337432, -4.500000000000000000, -3.000000000000000000 ) ) ;
#14934 = ORIENTED_EDGE ( 'NONE', *, *, #5054, .F. ) ;
#14933 = CARTESIAN_POINT ( 'NONE',  ( 2.002547531651519996, 10.57595306287302250, -6.845637710436074386 ) ) ;
#14935 = CARTESIAN_POINT ( 'NONE',  ( 0.4754618798421167414, -10.80499583390506402, -8.775436892861231186 ) ) ;
#14936 = CIRCLE ( 'NONE', #5765, 5.000000000000000888 ) ;
#14937 = EDGE_CURVE ( 'NONE', #4406, #10941, #13992, .T. ) ;
#14938 = VERTEX_POINT ( 'NONE', #4740 ) ;
#14939 = CARTESIAN_POINT ( 'NONE',  ( 8.438534575730034959, -6.454982381540305347, 2.341351102130253103 ) ) ;
#14940 = CARTESIAN_POINT ( 'NONE',  ( 0.3170788640506441158, 4.392045232375811459, 13.02120094575829867 ) ) ;
#14941 = ORIENTED_EDGE ( 'NONE', *, *, #8087, .F. ) ;
#14942 = ORIENTED_EDGE ( 'NONE', *, *, #13742, .F. ) ;
#14943 = DIRECTION ( 'NONE',  ( -0.000000000000000000, 1.000000000000000000, -0.000000000000000000 ) ) ;
#14944 = VECTOR ( 'NONE', #17380, 1000.000000000000000 ) ;
#14945 = VERTEX_POINT ( 'NONE', #6077 ) ;
#14946 = CARTESIAN_POINT ( 'NONE',  ( 16.56872352241294521, 0.004907101719995680782, 0.009207754980064214098 ) ) ;
#14947 = ORIENTED_EDGE ( 'NONE', *, *, #12876, .T. ) ;
#14948 = CARTESIAN_POINT ( 'NONE',  ( 8.522092701127531811, 6.722964936702098271, 1.786985377232055860 ) ) ;
#14949 = CYLINDRICAL_SURFACE ( 'NONE', #7493, 5.000000000000000000 ) ;
#14950 = CARTESIAN_POINT ( 'NONE',  ( 16.56872352241294521, 0.01033355228142499721, 0.001442253899401261912 ) ) ;
#14951 = FACE_OUTER_BOUND ( 'NONE', #2762, .T. ) ;
#14952 = CARTESIAN_POINT ( 'NONE',  ( 16.57778382496167424, 0.01466529584256784369, 0.002851818597094051173 ) ) ;
#14953 = CARTESIAN_POINT ( 'NONE',  ( 3.950837973638676281, 1.958075594453990487, -14.41405733518058341 ) ) ;
#14954 = EDGE_CURVE ( 'NONE', #2296, #11365, #16306, .T. ) ;
#14955 = CARTESIAN_POINT ( 'NONE',  ( 3.950837973638675393, -2.591948120961706792, -14.31366178983255466 ) ) ;
#14956 = CARTESIAN_POINT ( 'NONE',  ( -4.505465888036630062, -19.31487138727242581, 3.000000000000000000 ) ) ;
#14957 = CARTESIAN_POINT ( 'NONE',  ( 0.3132635586635958425, -12.89236642382225462, 4.743936529203192087 ) ) ;
#14958 = CARTESIAN_POINT ( 'NONE',  ( 1.847247051441594179, -11.78111530882020297, -4.004229874809150047 ) ) ;
#14959 = DIRECTION ( 'NONE',  ( 0.000000000000000000, -1.000000000000000000, 0.000000000000000000 ) ) ;
#14960 = B_SPLINE_CURVE_WITH_KNOTS ( 'NONE', 3,
 ( #10369, #10078, #8839, #15907, #17341, #18866 ),
 .UNSPECIFIED., .F., .F.,
 ( 4, 2, 4 ),
 ( 3.671973638477265170E-17, 0.0001825746017570593200, 0.0003651492035140796086 ),
 .UNSPECIFIED. ) ;
#14961 = ORIENTED_EDGE ( 'NONE', *, *, #10375, .T. ) ;
#14962 = ORIENTED_EDGE ( 'NONE', *, *, #16194, .F. ) ;
#14963 = ORIENTED_EDGE ( 'NONE', *, *, #6830, .T. ) ;
#14964 = ORIENTED_EDGE ( 'NONE', *, *, #462, .T. ) ;
#14965 = CARTESIAN_POINT ( 'NONE',  ( 2.002547531651519996, -9.778737580845639599, -7.942910686618280813 ) ) ;
#14966 = CARTESIAN_POINT ( 'NONE',  ( 2.636624412714134280, 2.862162146984768896, 15.80357026013147426 ) ) ;
#14967 =( BOUNDED_SURFACE ( )  B_SPLINE_SURFACE ( 3, 1, ( 
 ( #10947, #627 ),
 ( #2492, #9682 ),
 ( #980, #16764 ),
 ( #12457, #11036 ) ),
 .UNSPECIFIED., .F., .F., .T. ) 
 B_SPLINE_SURFACE_WITH_KNOTS ( ( 4, 4 ),
 ( 2, 2 ),
 ( 0.000000000000000000, 1.000000000000000000 ),
 ( 0.000000000000000000, 1.000000000000000000 ),
 .UNSPECIFIED. ) 
 GEOMETRIC_REPRESENTATION_ITEM ( )  RATIONAL_B_SPLINE_SURFACE ( (
 ( 1.000000000000000000, 1.000000000000000000),
 ( 0.7792777138730158093, 0.9689936506012928330),
 ( 0.7792777138730158093, 0.9689936506012928330),
 ( 1.000000000000000000, 1.000000000000000000) ) ) 
 REPRESENTATION_ITEM ( '' )  SURFACE ( )  );
#14968 = FACE_OUTER_BOUND ( 'NONE', #13168, .T. ) ;
#14969 = LINE ( 'NONE', #17849, #11741 ) ;
#14970 = AXIS2_PLACEMENT_3D ( 'NONE', #15761, #1237, #14335 ) ;
#14971 = CARTESIAN_POINT ( 'NONE',  ( 1.846138399168762101, -12.43476674860266940, 0.4167076046095114505 ) ) ;
#14972 = CARTESIAN_POINT ( 'NONE',  ( 3.512766787570837490, 10.40533104696128497, 10.87507422923887646 ) ) ;
#14973 = DIRECTION ( 'NONE',  ( 0.000000000000000000, 0.000000000000000000, 1.000000000000000000 ) ) ;
#14974 = CARTESIAN_POINT ( 'NONE',  ( 0.3151930723728398331, 8.013866567350898862, 11.16020735774769435 ) ) ;
#14975 = EDGE_CURVE ( 'NONE', #8559, #5701, #14761, .T. ) ;
#14976 = CARTESIAN_POINT ( 'NONE',  ( 1.847426409206449405, 0.01438352405959898543, -12.44303504652077841 ) ) ;
#14977 = EDGE_CURVE ( 'NONE', #5119, #18618, #10823, .T. ) ;
#14978 = CARTESIAN_POINT ( 'NONE',  ( 0.8740779401507027258, 13.83508928787419912, 3.609949156401401904 ) ) ;
#14979 = EDGE_CURVE ( 'NONE', #13788, #11580, #17404, .T. ) ;
#14980 = DIRECTION ( 'NONE',  ( -0.000000000000000000, -1.000000000000000000, -0.000000000000000000 ) ) ;
#14981 = DIRECTION ( 'NONE',  ( 0.000000000000000000, 0.000000000000000000, 1.000000000000000000 ) ) ;
#14982 = DIRECTION ( 'NONE',  ( 1.000000000000000000, 0.000000000000000000, 2.775557561562892929E-15 ) ) ;
#14983 = ORIENTED_EDGE ( 'NONE', *, *, #16559, .F. ) ;
#14984 = EDGE_LOOP ( 'NONE', ( #13655, #10318, #9620, #18460 ) ) ;
#14985 = VERTEX_POINT ( 'NONE', #11811 ) ;
#14986 = VERTEX_POINT ( 'NONE', #7520 ) ;
#14987 = DIRECTION ( 'NONE',  ( -1.000000000000000000, -0.000000000000000000, -0.000000000000000000 ) ) ;
#14988 = PLANE ( 'NONE',  #13577 ) ;
#14989 = AXIS2_PLACEMENT_3D ( 'NONE', #8039, #13847, #10807 ) ;
#14990 = CARTESIAN_POINT ( 'NONE',  ( 2.636624412717099908, 15.80357026013547816, -2.862162146981609201 ) ) ;
#14991 = CARTESIAN_POINT ( 'NONE',  ( 3.664313757352972711, 10.50730552161232545, 9.645155442698788661 ) ) ;
#14992 = CARTESIAN_POINT ( 'NONE',  ( -30.00000000000000355, -12.50000000000000178, -1.000000000000000000 ) ) ;
#14993 = VERTEX_POINT ( 'NONE', #3288 ) ;
#14994 = CARTESIAN_POINT ( 'NONE',  ( 1.847372867223022963, -3.945260592619128204, 11.80112642014553614 ) ) ;
#14995 = B_SPLINE_CURVE_WITH_KNOTS ( 'NONE', 3,
 ( #5240, #6687, #18330, #6499, #16997, #3902 ),
 .UNSPECIFIED., .F., .F.,
 ( 4, 2, 4 ),
 ( 5.421010862427522170E-19, 0.0001825746017570577750, 0.0003651492035141150078 ),
 .UNSPECIFIED. ) ;
#14996 = CARTESIAN_POINT ( 'NONE',  ( 0.3137051932979775248, -12.91601973349273891, 4.679953077377436266 ) ) ;
#14997 = CARTESIAN_POINT ( 'NONE',  ( -30.00000000000000355, -12.50000000000000178, 0.000000000000000000 ) ) ;
#14998 = CARTESIAN_POINT ( 'NONE',  ( 2.747332970342022840, 7.555624153089857131, -14.49942876448584173 ) ) ;
#14999 = FACE_OUTER_BOUND ( 'NONE', #1323, .T. ) ;
#15000 = CARTESIAN_POINT ( 'NONE',  ( 3.950837973638676281, 2.591948120962007884, -14.31366178983250670 ) ) ;
#15001 =( REPRESENTATION_RELATIONSHIP ('NONE','NONE', #5200, #12894 ) REPRESENTATION_RELATIONSHIP_WITH_TRANSFORMATION ( #12825 )SHAPE_REPRESENTATION_RELATIONSHIP( ) );
#15002 = VERTEX_POINT ( 'NONE', #10374 ) ;
#15003 = VECTOR ( 'NONE', #6895, 1000.000000000000000 ) ;
#15004 = EDGE_CURVE ( 'NONE', #2106, #3140, #4550, .T. ) ;
#15005 = CARTESIAN_POINT ( 'NONE',  ( 1.104287921197080512E-14, -7.013167318348350499, 25.01316734529528674 ) ) ;
#15007 = VERTEX_POINT ( 'NONE', #2895 ) ;
#15006 = CARTESIAN_POINT ( 'NONE',  ( 2.320521194583479829, -10.64885423995220393, -11.60169518685964363 ) ) ;
#15008 = CARTESIAN_POINT ( 'NONE',  ( 0.3137051932979792457, 12.91601973349270871, 4.679953077377533965 ) ) ;
#15009 = CARTESIAN_POINT ( 'NONE',  ( 0.3308579732647030647, -4.812490080619291177, 12.88563776947744088 ) ) ;
#15010 = EDGE_CURVE ( 'NONE', #13262, #8831, #13069, .T. ) ;
#15011 = ORIENTED_EDGE ( 'NONE', *, *, #5833, .T. ) ;
#15012 = LINE ( 'NONE', #14918, #460 ) ;
#15013 = PRODUCT ( 'socket button head screw_iso_ISO 7380 - M5 x 20 - 20C', 'socket button head screw_iso_ISO 7380 - M5 x 20 - 20C', '', ( #8266 ) ) ;
#15014 = CARTESIAN_POINT ( 'NONE',  ( 0.3286731010499749361, -6.995544057484789136, -12.00000000211884554 ) ) ;
#15015 = ORIENTED_EDGE ( 'NONE', *, *, #16712, .T. ) ;
#15016 = DIRECTION ( 'NONE',  ( 0.8320502943378440541, -0.5547001962252284812, 0.000000000000000000 ) ) ;
#15017 = CARTESIAN_POINT ( 'NONE',  ( 16.56782317627811096, -0.008141063682853442660, -0.005492611183757281634 ) ) ;
#15018 = CARTESIAN_POINT ( 'NONE',  ( 1.959212340397945118, 4.509090217468684436, -11.71715421693493830 ) ) ;
#15019 = CARTESIAN_POINT ( 'NONE',  ( 2.320520222537495680, -11.60169517779343096, -10.64885284335084847 ) ) ;
#15020 = VERTEX_POINT ( 'NONE', #9132 ) ;
#15021 = PRODUCT_DEFINITION ( 'UNKNOWN', '', #6238, #16519 ) ;
#15022 = TOROIDAL_SURFACE ( 'NONE', #13175, 3.499999999999992450, 0.5000000000000000000 ) ;
#15023 = ADVANCED_FACE ( 'NONE', ( #343 ), #3078, .F. ) ;
#15024 = CARTESIAN_POINT ( 'NONE',  ( 1.846138399168762101, -6.971848976711082280, 10.30487220521567693 ) ) ;
#15025 = CARTESIAN_POINT ( 'NONE',  ( 0.3148208552358953138, 11.24855514421875569, 7.888357771040743316 ) ) ;
#15026 = EDGE_CURVE ( 'NONE', #14770, #7599, #4184, .T. ) ;
#15027 = DIRECTION ( 'NONE',  ( -1.000000000000000000, 1.224646799147353454E-16, 0.000000000000000000 ) ) ;
#15029 = VERTEX_POINT ( 'NONE', #11047 ) ;
#15028 = CARTESIAN_POINT ( 'NONE',  ( 1.845755665166725068, 6.920419570228353301, 10.33920510797145909 ) ) ;
#15030 = CARTESIAN_POINT ( 'NONE',  ( 3.512766787570760663, -10.87507422923897238, 10.40533104696129918 ) ) ;
#15031 = B_SPLINE_CURVE_WITH_KNOTS ( 'NONE', 3,
 ( #14933, #3062, #13307, #8818, #14837, #17719 ),
 .UNSPECIFIED., .F., .F.,
 ( 4, 2, 4 ),
 ( 0.000000000000000000, 0.001500839035891550054, 0.003001678071783100109 ),
 .UNSPECIFIED. ) ;
#15032 = ORIENTED_EDGE ( 'NONE', *, *, #7806, .F. ) ;
#15033 = CARTESIAN_POINT ( 'NONE',  ( 3.950837973638677170, 13.10350451991849141, -6.316429227969337923 ) ) ;
#15034 = CARTESIAN_POINT ( 'NONE',  ( 2.353870697619111496, -12.92712089195302561, -0.7635393531607687079 ) ) ;
#15035 = ORIENTED_EDGE ( 'NONE', *, *, #3240, .F. ) ;
#15036 = ORIENTED_EDGE ( 'NONE', *, *, #14468, .F. ) ;
#15037 = LINE ( 'NONE', #523, #12758 ) ;
#15038 = VERTEX_POINT ( 'NONE', #4929 ) ;
#15039 = FACE_OUTER_BOUND ( 'NONE', #12450, .T. ) ;
#15040 = VERTEX_POINT ( 'NONE', #15155 ) ;
#15041 = CARTESIAN_POINT ( 'NONE',  ( 16.56782317627811096, -0.006045301465876687375, -0.007739510688078416953 ) ) ;
#15042 = EDGE_CURVE ( 'NONE', #4171, #15500, #16513, .T. ) ;
#15043 = SURFACE_STYLE_USAGE ( .BOTH. , #427 ) ;
#15044 = CARTESIAN_POINT ( 'NONE',  ( 16.56753206892534891, 0.004368917149004243779, -0.008432171035096398468 ) ) ;
#15045 = CARTESIAN_POINT ( 'NONE',  ( 0.3137051932979809665, 13.20008686438111312, -3.805684345189650042 ) ) ;
#15046 = AXIS2_PLACEMENT_3D ( 'NONE', #3954, #5384, #16860 ) ;
#15047 = LINE ( 'NONE', #5263, #2582 ) ;
#15048 = CARTESIAN_POINT ( 'NONE',  ( 0.4754618798421162973, -3.583352865732575943, -13.45049478164063395 ) ) ;
#15049 =( BOUNDED_SURFACE ( )  B_SPLINE_SURFACE ( 3, 1, ( 
 ( #13231, #4351 ),
 ( #10082, #10174 ),
 ( #147, #8841 ),
 ( #3083, #15999 ) ),
 .UNSPECIFIED., .F., .F., .T. ) 
 B_SPLINE_SURFACE_WITH_KNOTS ( ( 4, 4 ),
 ( 2, 2 ),
 ( 0.000000000000000000, 1.000000000000000000 ),
 ( 0.000000000000000000, 1.000000000000000000 ),
 .UNSPECIFIED. ) 
 GEOMETRIC_REPRESENTATION_ITEM ( )  RATIONAL_B_SPLINE_SURFACE ( (
 ( 1.000000000000000000, 1.000000000000000000),
 ( 0.7792777138730158093, 0.9689936506012928330),
 ( 0.7792777138730158093, 0.9689936506012928330),
 ( 1.000000000000000000, 1.000000000000000000) ) ) 
 REPRESENTATION_ITEM ( '' )  SURFACE ( )  );
#15050 = CARTESIAN_POINT ( 'NONE',  ( 1.845756295923363322, -10.33914852636099191, -6.920504327368305120 ) ) ;
#15051 = CARTESIAN_POINT ( 'NONE',  ( 0.3939822652208131992, -11.57634296752772229, 7.545099438011985349 ) ) ;
#15052 = LINE ( 'NONE', #9592, #18119 ) ;
#15053 = CARTESIAN_POINT ( 'NONE',  ( 2.500000000000000000, 0.000000000000000000, -3.000000000000000000 ) ) ;
#15054 = FACE_OUTER_BOUND ( 'NONE', #12270, .T. ) ;
#15055 =( LENGTH_UNIT ( ) NAMED_UNIT ( * ) SI_UNIT ( .MILLI., .METRE. ) );
#15056 = VERTEX_POINT ( 'NONE', #7998 ) ;
#15057 = VECTOR ( 'NONE', #9483, 1000.000000000000114 ) ;
#15058 = EDGE_LOOP ( 'NONE', ( #10330, #9349, #6359, #5725 ) ) ;
#15059 = ORIENTED_EDGE ( 'NONE', *, *, #5811, .T. ) ;
#15060 = B_SPLINE_CURVE_WITH_KNOTS ( 'NONE', 3,
 ( #15243, #2068, #15051, #9321, #10954, #12098 ),
 .UNSPECIFIED., .F., .F.,
 ( 4, 2, 4 ),
 ( 4.253224384355279651E-17, 0.0002014099069817287574, 0.0004028198139634150141 ),
 .UNSPECIFIED. ) ;
#15061 = VERTEX_POINT ( 'NONE', #1970 ) ;
#15062 = EDGE_CURVE ( 'NONE', #12290, #12155, #6271, .T. ) ;
#15063 = CARTESIAN_POINT ( 'NONE',  ( 0.4385251269669976359, -4.978066129061780032, 12.93791070501032436 ) ) ;
#15064 = CARTESIAN_POINT ( 'NONE',  ( -199.9999999999999716, -5.000000000000024869, 11.00000000000000000 ) ) ;
#15065 = CARTESIAN_POINT ( 'NONE',  ( 0.3137051932979809665, -4.679953077377580151, 12.91601973349268917 ) ) ;
#15066 = DIRECTION ( 'NONE',  ( -0.000000000000000000, 0.000000000000000000, 1.000000000000000000 ) ) ;
#15067 = CARTESIAN_POINT ( 'NONE',  ( 3.074695600507134419, -7.366518011945905720, -13.70113613813221676 ) ) ;
#15068 = CARTESIAN_POINT ( 'NONE',  ( -1.500000000000001332, 6.799999999999999822, 5.000000000000000000 ) ) ;
#15069 = LINE ( 'NONE', #6567, #18346 ) ;
#15070 = CARTESIAN_POINT ( 'NONE',  ( 2.705023505549863483, -3.294610156755986452, 12.88681800078731321 ) ) ;
#15071 = AXIS2_PLACEMENT_3D ( 'NONE', #3061, #14643, #1554 ) ;
#15072 = FACE_OUTER_BOUND ( 'NONE', #6297, .T. ) ;
#15073 = CARTESIAN_POINT ( 'NONE',  ( 2.002547531651519996, -10.57595306287296921, 6.845637710436153434 ) ) ;
#15074 = CIRCLE ( 'NONE', #5005, 5.000000000000000888 ) ;
#15075 = CARTESIAN_POINT ( 'NONE',  ( 0.4862570985993235340, -7.559321496869339185, -11.67702470553373750 ) ) ;
#15076 = CARTESIAN_POINT ( 'NONE',  ( 16.57210152137263393, -0.0006600038696348781500, -0.01453130299868639688 ) ) ;
#15077 = VERTEX_POINT ( 'NONE', #15053 ) ;
#15078 = B_SPLINE_CURVE_WITH_KNOTS ( 'NONE', 3,
 ( #15073, #2175, #16609, #13543, #9523, #18132 ),
 .UNSPECIFIED., .F., .F.,
 ( 4, 2, 4 ),
 ( 0.000000000000000000, 0.001500839035891550271, 0.003001678071783100542 ),
 .UNSPECIFIED. ) ;
#15079 = VERTEX_POINT ( 'NONE', #12467 ) ;
#15080 = ORIENTED_EDGE ( 'NONE', *, *, #16666, .T. ) ;
#15081 = ORIENTED_EDGE ( 'NONE', *, *, #5435, .T. ) ;
#15082 =( BOUNDED_SURFACE ( )  B_SPLINE_SURFACE ( 3, 1, ( 
 ( #8825, #7405 ),
 ( #13215, #5657 ),
 ( #8546, #133 ),
 ( #4152, #9972 ) ),
 .UNSPECIFIED., .F., .F., .T. ) 
 B_SPLINE_SURFACE_WITH_KNOTS ( ( 4, 4 ),
 ( 2, 2 ),
 ( 0.000000000000000000, 1.000000000000000000 ),
 ( 0.000000000000000000, 1.000000000000000000 ),
 .UNSPECIFIED. ) 
 GEOMETRIC_REPRESENTATION_ITEM ( )  RATIONAL_B_SPLINE_SURFACE ( (
 ( 1.000000000000000000, 1.000000000000000000),
 ( 0.9593108457356467333, 0.9995965569486454649),
 ( 0.9593108457356467333, 0.9995965569486454649),
 ( 1.000000000000000000, 1.000000000000000000) ) ) 
 REPRESENTATION_ITEM ( '' )  SURFACE ( )  );
#15083 = CARTESIAN_POINT ( 'NONE',  ( 1.846138399168762101, -6.971848976710933954, -10.30487220521577818 ) ) ;
#15084 = EDGE_CURVE ( 'NONE', #8361, #11620, #3700, .T. ) ;
#15085 = EDGE_CURVE ( 'NONE', #4150, #15496, #18522, .T. ) ;
#15086 = EDGE_CURVE ( 'NONE', #2621, #9990, #16710, .T. ) ;
#15087 = DIRECTION ( 'NONE',  ( 0.000000000000000000, -1.000000000000000000, 0.000000000000000000 ) ) ;
#15088 = VECTOR ( 'NONE', #7844, 1000.000000000000114 ) ;
#15089 = LINE ( 'NONE', #6304, #16928 ) ;
#15090 = CARTESIAN_POINT ( 'NONE',  ( 3.950837973638675393, 10.51028938476217967, 10.05648675950130233 ) ) ;
#15091 = PRODUCT_DEFINITION_FORMATION_WITH_SPECIFIED_SOURCE ( 'ANY', '', #537, .NOT_KNOWN. ) ;
#15092 = DIRECTION ( 'NONE',  ( 0.000000000000000000, 0.000000000000000000, -1.000000000000000000 ) ) ;
#15093 = VERTEX_POINT ( 'NONE', #10956 ) ;
#15094 = CARTESIAN_POINT ( 'NONE',  ( -6.236214402462488593, 7.499999999999999112, -17.00000000000000355 ) ) ;
#15095 = CARTESIAN_POINT ( 'NONE',  ( 1.846138399168762989, 11.69739621335922308, 4.238866729160444713 ) ) ;
#15096 = CARTESIAN_POINT ( 'NONE',  ( -1.391479049022228187, 7.499999999999999112, -14.80352021213800917 ) ) ;
#15097 = CARTESIAN_POINT ( 'NONE',  ( 16.56872352241294521, -0.009207754980064163791, 0.004907101719995779661 ) ) ;
#15098 = CARTESIAN_POINT ( 'NONE',  ( 16.56822296793089322, -0.008619100080558715279, 0.005339139727952894703 ) ) ;
#15099 = CARTESIAN_POINT ( 'NONE',  ( 0.4754618798421167414, 12.98792082933644743, 5.007009103465293265 ) ) ;
#15100 = CARTESIAN_POINT ( 'NONE',  ( 2.002547531651519996, -3.242439124566566910, -12.17374746633581495 ) ) ;
#15101 = EDGE_CURVE ( 'NONE', #3664, #15826, #7812, .T. ) ;
#15102 = CIRCLE ( 'NONE', #1668, 5.000000000000000888 ) ;
#15103 = VERTEX_POINT ( 'NONE', #439 ) ;
#15104 = CARTESIAN_POINT ( 'NONE',  ( 16.57210152137263393, 0.01453130299868640209, -0.0006600038696348341314 ) ) ;
#15106 = ORIENTED_EDGE ( 'NONE', *, *, #12217, .F. ) ;
#15105 = CARTESIAN_POINT ( 'NONE',  ( 1.847372867223030068, 11.86627781945713167, -3.744745203533853317 ) ) ;
#15107 = CARTESIAN_POINT ( 'NONE',  ( 3.377929128793397684, -10.50432311212909475, 9.234024516648283054 ) ) ;
#15108 = AXIS2_PLACEMENT_3D ( 'NONE', #10020, #8322, #15855 ) ;
#15109 = AXIS2_PLACEMENT_3D ( 'NONE', #16143, #11939, #3422 ) ;
#15110 = CARTESIAN_POINT ( 'NONE',  ( 16.56872352241294521, -0.001442253899401298341, 0.01033355228142499027 ) ) ;
#15111 = ORIENTED_EDGE ( 'NONE', *, *, #8543, .T. ) ;
#15112 = LINE ( 'NONE', #12060, #10256 ) ;
#15113 = CARTESIAN_POINT ( 'NONE',  ( -4.153045036173530491, -5.656186534233802021, -12.00000000830646840 ) ) ;
#15114 = ORIENTED_EDGE ( 'NONE', *, *, #2429, .F. ) ;
#15115 = FACE_OUTER_BOUND ( 'NONE', #18807, .T. ) ;
#15116 = CARTESIAN_POINT ( 'NONE',  ( 0.3151926232592509591, 13.73922722301401400, -0.07678256780562460471 ) ) ;
#15117 = EDGE_CURVE ( 'NONE', #16909, #5705, #4840, .T. ) ;
#15118 = AXIS2_PLACEMENT_3D ( 'NONE', #16949, #9498, #14079 ) ;
#15119 = CARTESIAN_POINT ( 'NONE',  ( 0.4384471787762852513, 7.540925784514715957, -11.63197976518319798 ) ) ;
#15120 = AXIS2_PLACEMENT_3D ( 'NONE', #12567, #4161, #16973 ) ;
#15121 = DIRECTION ( 'NONE',  ( 0.000000000000000000, -0.5000000000000003331, 0.8660254037844383745 ) ) ;
#15122 = B_SPLINE_CURVE_WITH_KNOTS ( 'NONE', 3,
 ( #18380, #1437, #11130, #16856, #18904, #3763, #16769, #3670, #15510, #8693, #12463, #16951, #18721 ),
 .UNSPECIFIED., .F., .F.,
 ( 4, 3, 3, 3, 4 ),
 ( 0.000000000000000000, 0.0002299804304191501543, 0.0004599608082120262018, 0.0006467586077648019086, 0.0008336169836825998080 ),
 .UNSPECIFIED. ) ;
#15123 = VECTOR ( 'NONE', #8686, 1000.000000000000000 ) ;
#15124 = ORIENTED_EDGE ( 'NONE', *, *, #14666, .T. ) ;
#15125 = B_SPLINE_CURVE_WITH_KNOTS ( 'NONE', 3,
 ( #16422, #3006, #6286, #10685 ),
 .UNSPECIFIED., .F., .F.,
 ( 4, 4 ),
 ( 1.330347433792404293E-17, 0.003005512676784847462 ),
 .UNSPECIFIED. ) ;
#15126 = EDGE_CURVE ( 'NONE', #8563, #17236, #13956, .T. ) ;
#15127 = DIRECTION ( 'NONE',  ( 0.8629742774544859607, -0.5052478564545405115, -0.000000000000000000 ) ) ;
#15128 = LINE ( 'NONE', #14932, #7999 ) ;
#15130 = EDGE_LOOP ( 'NONE', ( #1757, #16492, #18048, #6878 ) ) ;
#15129 = CARTESIAN_POINT ( 'NONE',  ( 0.3095370825347233956, -0.4597470195089253808, -13.73357284481725316 ) ) ;
#15131 = DIRECTION ( 'NONE',  ( 1.000000000000000000, 0.000000000000000000, 0.000000000000000000 ) ) ;
#15132 = VECTOR ( 'NONE', #11477, 1000.000000000000000 ) ;
#15133 = FACE_OUTER_BOUND ( 'NONE', #18483, .T. ) ;
#15134 = CARTESIAN_POINT ( 'NONE',  ( 2.636624412715138366, -15.91454522070249311, -2.161493821597819665 ) ) ;
#15135 = CARTESIAN_POINT ( 'NONE',  ( 5.000000000000000000, 0.000000000000000000, 0.000000000000000000 ) ) ;
#15136 = EDGE_LOOP ( 'NONE', ( #947, #11223, #1498, #18809 ) ) ;
#15137 = ORIENTED_EDGE ( 'NONE', *, *, #16443, .F. ) ;
#15138 = CYLINDRICAL_SURFACE ( 'NONE', #13380, 5.000000000000049738 ) ;
#15139 = EDGE_LOOP ( 'NONE', ( #2437, #7982, #18715, #417 ) ) ;
#15140 = CARTESIAN_POINT ( 'NONE',  ( 3.950837973638676281, 12.81214529934975310, 6.888253895133341409 ) ) ;
#15141 = ORIENTED_EDGE ( 'NONE', *, *, #16559, .T. ) ;
#15142 = DIRECTION ( 'NONE',  ( 1.000000000000000000, 1.298018465182616140E-16, -0.000000000000000000 ) ) ;
#15143 = CARTESIAN_POINT ( 'NONE',  ( 8.438534575730034959, 6.598402093327905504, -1.899950616255119407 ) ) ;
#15144 = CARTESIAN_POINT ( 'NONE',  ( 16.56782317627811096, 0.008141063682853404496, 0.005492611183757338013 ) ) ;
#15145 = CARTESIAN_POINT ( 'NONE',  ( 1.254255976357524505, -1.011593778944422262, 14.64488542023450535 ) ) ;
#15146 = CARTESIAN_POINT ( 'NONE',  ( -26.50000000000000711, -12.50000000000000178, -0.5000000000000000000 ) ) ;
#15147 = CARTESIAN_POINT ( 'NONE',  ( 0.4385251269669978025, 12.93791070501034390, 4.978066129061732070 ) ) ;
#15148 = FACE_OUTER_BOUND ( 'NONE', #4287, .T. ) ;
#15149 = COLOUR_RGB ( '', 0.08235294, 0.09019608, 0.10196078) ;
#15150 = EDGE_CURVE ( 'NONE', #11214, #12864, #7615, .T. ) ;
#15151 = AXIS2_PLACEMENT_3D ( 'NONE', #9578, #15409, #18456 ) ;
#15152 = CARTESIAN_POINT ( 'NONE',  ( 0.3132642857406495174, 0.5276792104584192566, -13.72733058964894681 ) ) ;
#15153 = ORIENTED_EDGE ( 'NONE', *, *, #12977, .F. ) ;
#15154 = CARTESIAN_POINT ( 'NONE',  ( 1.847034903785823357, 7.498375632854758166, -9.929438108952064468 ) ) ;
#15155 = CARTESIAN_POINT ( 'NONE',  ( 2.369999999999999662, -4.750000000000000888, -5.817072295949926440E-16 ) ) ;
#15156 = EDGE_CURVE ( 'NONE', #1137, #3637, #8166, .T. ) ;
#15157 = CARTESIAN_POINT ( 'NONE',  ( 20.00000000000000000, -2.500000000000000444, -12.00000000000000000 ) ) ;
#15158 = CARTESIAN_POINT ( 'NONE',  ( 0.3095370825347224519, -3.806662003783507497, 13.20347358821913275 ) ) ;
#15159 = EDGE_LOOP ( 'NONE', ( #2866, #9762, #5229, #1805 ) ) ;
#15160 = ORIENTED_EDGE ( 'NONE', *, *, #15381, .T. ) ;
#15161 = ORIENTED_EDGE ( 'NONE', *, *, #2636, .T. ) ;
#15162 = VERTEX_POINT ( 'NONE', #16864 ) ;
#15163 = B_SPLINE_CURVE_WITH_KNOTS ( 'NONE', 3,
 ( #17947, #14771, #10582, #4847, #258, #16012, #7630, #6181, #11309, #15683, #11122, #3849, #14265 ),
 .UNSPECIFIED., .F., .F.,
 ( 4, 3, 3, 3, 4 ),
 ( 2.453269466693398698E-18, 0.0002299780670421062274, 0.0004599561239687902829, 0.0006896788984287884972, 0.0009194956271626412558 ),
 .UNSPECIFIED. ) ;
#15164 = VERTEX_POINT ( 'NONE', #12200 ) ;
#15165 = CARTESIAN_POINT ( 'NONE',  ( 1.846524061778018311, -12.43723828841088341, -0.3544704288993787422 ) ) ;
#15166 =( BOUNDED_SURFACE ( )  B_SPLINE_SURFACE ( 3, 1, ( 
 ( #3787, #7274 ),
 ( #15952, #5814 ),
 ( #14521, #2840 ),
 ( #17104, #18015 ) ),
 .UNSPECIFIED., .F., .F., .T. ) 
 B_SPLINE_SURFACE_WITH_KNOTS ( ( 4, 4 ),
 ( 2, 2 ),
 ( 0.000000000000000000, 1.000000000000000000 ),
 ( 0.000000000000000000, 1.000000000000000000 ),
 .UNSPECIFIED. ) 
 GEOMETRIC_REPRESENTATION_ITEM ( )  RATIONAL_B_SPLINE_SURFACE ( (
 ( 1.000000000000000000, 1.000000000000000000),
 ( 0.9593108457356467333, 0.9995965569486454649),
 ( 0.9593108457356467333, 0.9995965569486454649),
 ( 1.000000000000000000, 1.000000000000000000) ) ) 
 REPRESENTATION_ITEM ( '' )  SURFACE ( )  );
#15167 = CARTESIAN_POINT ( 'NONE',  ( 16.56872352241294521, 0.01033355228142499721, 0.001442253899401261912 ) ) ;
#15168 = CARTESIAN_POINT ( 'NONE',  ( 1.846138399168762101, 9.815003036200520725, -7.646096044339786069 ) ) ;
#15169 = PRODUCT_DEFINITION_CONTEXT ( 'detailed design', #14485, 'design' ) ;
#15170 = AXIS2_PLACEMENT_3D ( 'NONE', #5871, #18343, #16908 ) ;
#15171 = LINE ( 'NONE', #16876, #16777 ) ;
#15172 = CIRCLE ( 'NONE', #13646, 16.06066017081991149 ) ;
#15173 = ADVANCED_FACE ( 'NONE', ( #16593 ), #2160, .F. ) ;
#15174 = CIRCLE ( 'NONE', #7246, 1.500000000000000000 ) ;
#15175 = CARTESIAN_POINT ( 'NONE',  ( 20.00000000000000000, -7.500000000000000888, -16.99999999999999645 ) ) ;
#15176 = CARTESIAN_POINT ( 'NONE',  ( 2.636624412717099908, 15.80357026013547816, -2.862162146981609201 ) ) ;
#15177 = DIRECTION ( 'NONE',  ( -1.000000000000000000, -0.000000000000000000, -0.000000000000000000 ) ) ;
#15178 =( GEOMETRIC_REPRESENTATION_CONTEXT ( 3 ) GLOBAL_UNCERTAINTY_ASSIGNED_CONTEXT ( ( #8838 ) ) GLOBAL_UNIT_ASSIGNED_CONTEXT ( ( #13694, #410, #18544 ) ) REPRESENTATION_CONTEXT ( 'NONE', 'WORKASPACE' ) );
#15179 = DIRECTION ( 'NONE',  ( 0.000000000000000000, 0.000000000000000000, 1.000000000000000000 ) ) ;
#15180 = VECTOR ( 'NONE', #15638, 1000.000000000000000 ) ;
#15181 = AXIS2_PLACEMENT_3D ( 'NONE', #11776, #4230, #4515 ) ;
#15182 = EDGE_CURVE ( 'NONE', #3563, #2803, #8449, .T. ) ;
#15183 = ORIENTED_EDGE ( 'NONE', *, *, #7772, .F. ) ;
#15184 = ORIENTED_EDGE ( 'NONE', *, *, #9213, .T. ) ;
#15185 = ORIENTED_EDGE ( 'NONE', *, *, #7188, .F. ) ;
#15186 = AXIS2_PLACEMENT_3D ( 'NONE', #13524, #7814, #17744 ) ;
#15187 = ORIENTED_EDGE ( 'NONE', *, *, #11689, .T. ) ;
#15188 = DIRECTION ( 'NONE',  ( -1.000000000000000000, -0.000000000000000000, -0.000000000000000000 ) ) ;
#15189 = AXIS2_PLACEMENT_3D ( 'NONE', #8064, #789, #3364 ) ;
#15190 = CARTESIAN_POINT ( 'NONE',  ( 16.58200780006414732, 0.01041078477703982763, -0.004047297414157931088 ) ) ;
#15191 = CARTESIAN_POINT ( 'NONE',  ( 1.847380140988736708, -7.402792205949027426, -10.00162556679659076 ) ) ;
#15192 = DIRECTION ( 'NONE',  ( 0.000000000000000000, 0.000000000000000000, -1.000000000000000000 ) ) ;
#15193 = CARTESIAN_POINT ( 'NONE',  ( 2.636624412715137922, 2.161493821597615828, 15.91454522070216093 ) ) ;
#15194 = ORIENTED_EDGE ( 'NONE', *, *, #14876, .T. ) ;
#15195 = CARTESIAN_POINT ( 'NONE',  ( 1.846138399168762989, 9.815003036200414144, 7.646096044339929954 ) ) ;
#15196 = CARTESIAN_POINT ( 'NONE',  ( 2.636624412714237309, 7.605649742761960042, 14.14563173255213613 ) ) ;
#15197 = CARTESIAN_POINT ( 'NONE',  ( -0.1174197124920530882, 7.499999999999999112, -14.18273494860542705 ) ) ;
#15198 = CARTESIAN_POINT ( 'NONE',  ( 1.847461586945732703, -10.04711372545050097, 7.341074796295904648 ) ) ;
#15199 = VECTOR ( 'NONE', #14196, 1000.000000000000000 ) ;
#15200 = CARTESIAN_POINT ( 'NONE',  ( 20.00000000000000000, 0.000000000000000000, -16.99999999999999645 ) ) ;
#15201 = CARTESIAN_POINT ( 'NONE',  ( 3.950837973638676281, -6.888253895133199300, -12.81214529934982949 ) ) ;
#15202 = B_SPLINE_CURVE_WITH_KNOTS ( 'NONE', 3,
 ( #9462, #15284, #4467, #16129 ),
 .UNSPECIFIED., .F., .F.,
 ( 4, 4 ),
 ( 9.204257061898183523E-17, 0.002004993803842712065 ),
 .UNSPECIFIED. ) ;
#15203 = DIRECTION ( 'NONE',  ( -1.000000000000000000, -0.000000000000000000, -0.000000000000000000 ) ) ;
#15204 = EDGE_CURVE ( 'NONE', #2316, #15038, #8357, .T. ) ;
#15205 = ORIENTED_EDGE ( 'NONE', *, *, #17148, .F. ) ;
#15207 = EDGE_LOOP ( 'NONE', ( #5338, #13390, #7525, #9355 ) ) ;
#15206 = CARTESIAN_POINT ( 'NONE',  ( 16.58200780006414732, 0.0006320991582340733123, 0.01115192838421469670 ) ) ;
#15208 = FACE_OUTER_BOUND ( 'NONE', #9304, .T. ) ;
#15209 = VECTOR ( 'NONE', #14320, 1000.000000000000000 ) ;
#15210 = ORIENTED_EDGE ( 'NONE', *, *, #15319, .T. ) ;
#15211 = CARTESIAN_POINT ( 'NONE',  ( 3.950837973638668288, 14.41405733518061538, -1.958075594453841273 ) ) ;
#15212 = CARTESIAN_POINT ( 'NONE',  ( -2.037104019874120375, -6.699095661347423736, -11.99999999578283294 ) ) ;
#15213 = ORIENTED_EDGE ( 'NONE', *, *, #15403, .T. ) ;
#15214 = CARTESIAN_POINT ( 'NONE',  ( 0.3170788640506441158, 13.02120094575834131, -4.392045232375677344 ) ) ;
#15215 = CARTESIAN_POINT ( 'NONE',  ( 3.950837973638675393, 6.888253895133479965, -12.81214529934967672 ) ) ;
#15216 = CARTESIAN_POINT ( 'NONE',  ( 1.918921323896321862, -11.69058285425787247, -4.466082741316331983 ) ) ;
#15217 = CARTESIAN_POINT ( 'NONE',  ( 0.4862570985993235340, 13.89016912371017476, 0.7479633556562934604 ) ) ;
#15218 = CONICAL_SURFACE ( 'NONE', #16746, 2.100000000000000977, 1.029744258676656532 ) ;
#15219 = EDGE_CURVE ( 'NONE', #12360, #4507, #12926, .T. ) ;
#15220 = ADVANCED_FACE ( 'NONE', ( #9774 ), #14820, .F. ) ;
#15221 = CARTESIAN_POINT ( 'NONE',  ( 16.58200780006414732, -0.008650561019685578876, 0.007066318000004673597 ) ) ;
#15222 = EDGE_CURVE ( 'NONE', #5564, #1182, #6639, .T. ) ;
#15223 = CARTESIAN_POINT ( 'NONE',  ( 0.000000000000000000, 3.061616997868382648E-16, -2.499999999999999556 ) ) ;
#15225 = ORIENTED_EDGE ( 'NONE', *, *, #11190, .F. ) ;
#15224 = DIRECTION ( 'NONE',  ( 1.540743955509788340E-33, 1.000000000000000000, 2.533398541561209262E-17 ) ) ;
#15226 = CARTESIAN_POINT ( 'NONE',  ( 16.56753206892534891, -0.009389754735542259201, -0.001421777558675912110 ) ) ;
#15227 = ORIENTED_EDGE ( 'NONE', *, *, #13273, .F. ) ;
#15228 = CARTESIAN_POINT ( 'NONE',  ( 0.3142011359265350912, -11.33549115679417696, -7.762194356530893735 ) ) ;
#15229 = CARTESIAN_POINT ( 'NONE',  ( -20.00000000000000000, -2.500000000000000444, -12.00000000000000000 ) ) ;
#15230 = VERTEX_POINT ( 'NONE', #1080 ) ;
#15231 = VERTEX_POINT ( 'NONE', #6746 ) ;
#15232 = CARTESIAN_POINT ( 'NONE',  ( 0.3142014840576516921, 11.33546131209473806, -7.762239086932731347 ) ) ;
#15233 = CARTESIAN_POINT ( 'NONE',  ( 3.950837973638668288, 0.000000000000000000, 0.000000000000000000 ) ) ;
#15234 = ORIENTED_EDGE ( 'NONE', *, *, #721, .F. ) ;
#15235 = DIRECTION ( 'NONE',  ( -1.000000000000000000, -0.000000000000000000, -0.000000000000000000 ) ) ;
#15236 =( NAMED_UNIT ( * ) SI_UNIT ( $, .STERADIAN. ) SOLID_ANGLE_UNIT ( ) );
#15237 = LINE ( 'NONE', #16674, #4422 ) ;
#15238 = DIRECTION ( 'NONE',  ( -0.7071067811865486830, 0.000000000000000000, 0.7071067811865464625 ) ) ;
#15239 = CARTESIAN_POINT ( 'NONE',  ( 16.56872352241294521, 0.004907101719995680782, 0.009207754980064214098 ) ) ;
#15240 = PRODUCT_CONTEXT ( 'NONE', #5094, 'mechanical' ) ;
#15241 = SURFACE_STYLE_FILL_AREA ( #18202 ) ;
#15242 = CARTESIAN_POINT ( 'NONE',  ( 16.56822296793089322, -0.009847136207495329335, 0.002414375228568802195 ) ) ;
#15243 = CARTESIAN_POINT ( 'NONE',  ( 0.4862570985993235340, -11.67702470553370553, 7.559321496869385371 ) ) ;
#15244 = CARTESIAN_POINT ( 'NONE',  ( 3.950837973638676281, -10.05648675950133963, 10.51028938476214059 ) ) ;
#15245 = CARTESIAN_POINT ( 'NONE',  ( 0.4862570985993235340, 8.769551628660735787, 10.79774104611376373 ) ) ;
#15246 = EDGE_CURVE ( 'NONE', #7506, #15077, #5294, .T. ) ;
#15247 = LINE ( 'NONE', #6748, #3584 ) ;
#15248 = CARTESIAN_POINT ( 'NONE',  ( 0.4384471787762798112, -7.540925784514636909, 11.63197976518326371 ) ) ;
#15249 = CIRCLE ( 'NONE', #16155, 14.54644660717763927 ) ;
#15250 = ORIENTED_EDGE ( 'NONE', *, *, #1001, .F. ) ;
#15251 = AXIS2_PLACEMENT_3D ( 'NONE', #3053, #11872, #2770 ) ;
#15252 = VERTEX_POINT ( 'NONE', #11136 ) ;
#15253 = ORIENTED_EDGE ( 'NONE', *, *, #15375, .T. ) ;
#15254 = ORIENTED_EDGE ( 'NONE', *, *, #12954, .T. ) ;
#15255 = ORIENTED_EDGE ( 'NONE', *, *, #7287, .T. ) ;
#15256 = MECHANICAL_DESIGN_GEOMETRIC_PRESENTATION_REPRESENTATION (  '', ( #8236 ), #4882 ) ;
#15257 = LINE ( 'NONE', #18308, #13305 ) ;
#15258 = CARTESIAN_POINT ( 'NONE',  ( 0.3448739086965406653, -7.500000000000000888, -14.22069309503974921 ) ) ;
#15259 = ADVANCED_FACE ( 'NONE', ( #4146 ), #2469, .F. ) ;
#15260 = CARTESIAN_POINT ( 'NONE',  ( 2.320520222538070776, 1.795797593769018485, -15.64520721754711730 ) ) ;
#15261 = DIRECTION ( 'NONE',  ( 1.000000000000000000, 0.000000000000000000, 0.000000000000000000 ) ) ;
#15262 = CARTESIAN_POINT ( 'NONE',  ( -4.999999999999995559, -30.00000000000000000, 31.00000000000000000 ) ) ;
#15263 = CARTESIAN_POINT ( 'NONE',  ( 0.4384471787762840855, 12.93784327393180433, -4.978024343488911541 ) ) ;
#15264 = CARTESIAN_POINT ( 'NONE',  ( 0.3170788640506440603, -0.1533108587037102788, 13.74111462631963576 ) ) ;
#15265 = EDGE_CURVE ( 'NONE', #8358, #12958, #8538, .T. ) ;
#15266 = CARTESIAN_POINT ( 'NONE',  ( 2.320521194582656044, -11.60169518685945356, 10.64885423995117542 ) ) ;
#15267 = EDGE_CURVE ( 'NONE', #10542, #6415, #1744, .T. ) ;
#15268 = CARTESIAN_POINT ( 'NONE',  ( 0.3095370825347233956, -11.38092634279623105, -7.700448427571997101 ) ) ;
#15269 = ORIENTED_EDGE ( 'NONE', *, *, #5210, .F. ) ;
#15270 = EDGE_CURVE ( 'NONE', #3148, #3596, #9068, .T. ) ;
#15271 = VERTEX_POINT ( 'NONE', #7019 ) ;
#15272 = ORIENTED_EDGE ( 'NONE', *, *, #11689, .F. ) ;
#15273 = ORIENTED_EDGE ( 'NONE', *, *, #5347, .T. ) ;
#15274 = LINE ( 'NONE', #7938, #3091 ) ;
#15275 = CARTESIAN_POINT ( 'NONE',  ( 2.747332970342022840, 14.49942876448603180, -7.555624153089486761 ) ) ;
#15276 = CARTESIAN_POINT ( 'NONE',  ( 3.074695600507765025, 15.30693405987741684, -2.772091048738999142 ) ) ;
#15277 = CARTESIAN_POINT ( 'NONE',  ( 16.56753206892534891, 0.008432171035096448775, -0.004368917149005361808 ) ) ;
#15278 = CARTESIAN_POINT ( 'NONE',  ( 0.3939875929385642239, 13.34133634968955917, 3.598491969338272867 ) ) ;
#15279 = VERTEX_POINT ( 'NONE', #12555 ) ;
#15280 = CARTESIAN_POINT ( 'NONE',  ( 0.3720661004400037664, 8.694226082900744501, -10.73619472937692620 ) ) ;
#15281 = EDGE_CURVE ( 'NONE', #15038, #14303, #11512, .T. ) ;
#15282 = LINE ( 'NONE', #2193, #17204 ) ;
#15283 = CARTESIAN_POINT ( 'NONE',  ( -3.669726844813804956, 7.500000000000255795, -13.21471411064774237 ) ) ;
#15284 = CARTESIAN_POINT ( 'NONE',  ( 3.074695600507423521, -10.75417554975728329, -11.23985886659437483 ) ) ;
#15285 = B_SPLINE_CURVE_WITH_KNOTS ( 'NONE', 3,
 ( #3650, #12071, #9197, #10829, #2037, #15024 ),
 .UNSPECIFIED., .F., .F.,
 ( 4, 2, 4 ),
 ( 3.303099811781675862E-17, 0.0001825746017570575581, 0.0003651492035140820481 ),
 .UNSPECIFIED. ) ;
#15286 = DIRECTION ( 'NONE',  ( 1.000000000000000000, 0.000000000000000000, 0.000000000000000000 ) ) ;
#15287 = EDGE_CURVE ( 'NONE', #14370, #13171, #3258, .T. ) ;
#15288 = CARTESIAN_POINT ( 'NONE',  ( 0.3137051932979757485, 12.91601973349276733, -4.679953077377353665 ) ) ;
#15289 = ORIENTED_EDGE ( 'NONE', *, *, #949, .T. ) ;
#15291 = ORIENTED_EDGE ( 'NONE', *, *, #1186, .T. ) ;
#15290 = CARTESIAN_POINT ( 'NONE',  ( 4.336808689942017736E-15, -27.00000000000000000, 31.00000000000000000 ) ) ;
#15292 = CARTESIAN_POINT ( 'NONE',  ( -194.9999999999999716, -25.00000000000003197, 3.000000000000000000 ) ) ;
#15293 = AXIS2_PLACEMENT_3D ( 'NONE', #10595, #16330, #7644 ) ;
#15294 = ORIENTED_EDGE ( 'NONE', *, *, #3630, .F. ) ;
#15295 = CARTESIAN_POINT ( 'NONE',  ( 16.56782317627811096, -0.003357783021327886107, -0.009228812961908644183 ) ) ;
#15296 = CARTESIAN_POINT ( 'NONE',  ( -5.616333669597630696, -4.188188789804105916, -12.00000000261157496 ) ) ;
#15297 = ORIENTED_EDGE ( 'NONE', *, *, #2619, .F. ) ;
#15298 = CARTESIAN_POINT ( 'NONE',  ( 1.560000000000000053, -1.732050807568877859, -1.752539433813135784E-17 ) ) ;
#15299 = ADVANCED_FACE ( 'NONE', ( #12743 ), #5557, .T. ) ;
#15300 = DIRECTION ( 'NONE',  ( -1.000000000000000000, 0.000000000000000000, 0.000000000000000000 ) ) ;
#15301 = CARTESIAN_POINT ( 'NONE',  ( 2.320521194582656932, -15.64520804578280888, 1.795798718313643683 ) ) ;
#15302 = CARTESIAN_POINT ( 'NONE',  ( 2.636624412714236865, 0.000000000000000000, 0.000000000000000000 ) ) ;
#15303 = CIRCLE ( 'NONE', #4626, 2.499999999999995115 ) ;
#15304 = CARTESIAN_POINT ( 'NONE',  ( 0.4754618798421171855, -13.45049478164057000, -3.583352865732813530 ) ) ;
#15305 = B_SPLINE_CURVE_WITH_KNOTS ( 'NONE', 3,
 ( #14841, #8728, #4721, #16286 ),
 .UNSPECIFIED., .F., .F.,
 ( 4, 4 ),
 ( 4.336808689942017736E-19, 0.003005512676784827947 ),
 .UNSPECIFIED. ) ;
#15306 = DIRECTION ( 'NONE',  ( 0.000000000000000000, 0.000000000000000000, 1.000000000000000000 ) ) ;
#15308 = ORIENTED_EDGE ( 'NONE', *, *, #18238, .T. ) ;
#15307 = CARTESIAN_POINT ( 'NONE',  ( 1.321128355694181398E-14, -7.013167318348350499, 25.01316734529530095 ) ) ;
#15309 = DIRECTION ( 'NONE',  ( 1.000000000000000000, 0.000000000000000000, -0.000000000000000000 ) ) ;
#15310 = CARTESIAN_POINT ( 'NONE',  ( 16.56679352167444819, -0.001390132774594504727, 0.009190982326619714232 ) ) ;
#15311 = FACE_OUTER_BOUND ( 'NONE', #3685, .T. ) ;
#15312 = CYLINDRICAL_SURFACE ( 'NONE', #16411, 1.000000000000000000 ) ;
#15313 = ORIENTED_EDGE ( 'NONE', *, *, #14086, .F. ) ;
#15314 = ORIENTED_EDGE ( 'NONE', *, *, #7372, .T. ) ;
#15315 = CARTESIAN_POINT ( 'NONE',  ( 2.002547531651519996, 4.532360870844494016, -11.75462648437097180 ) ) ;
#15316 = FACE_OUTER_BOUND ( 'NONE', #16211, .T. ) ;
#15317 = ORIENTED_EDGE ( 'NONE', *, *, #14897, .T. ) ;
#15318 = ADVANCED_FACE ( 'NONE', ( #17137 ), #4048, .F. ) ;
#15319 = EDGE_CURVE ( 'NONE', #10123, #11928, #2972, .T. ) ;
#15320 = EDGE_CURVE ( 'NONE', #5117, #1184, #16011, .T. ) ;
#15321 = CARTESIAN_POINT ( 'NONE',  ( 16.56753206892534891, 0.008432171035096382855, 0.004368917149004273269 ) ) ;
#15322 = CARTESIAN_POINT ( 'NONE',  ( 0.3720661004400037664, -11.58636699658219982, 7.524064345033424139 ) ) ;
#15323 = VECTOR ( 'NONE', #8891, 1000.000000000000000 ) ;
#15324 = CARTESIAN_POINT ( 'NONE',  ( -31.48433267924924550, 17.77350098112614418, 0.000000000000000000 ) ) ;
#15325 = CARTESIAN_POINT ( 'NONE',  ( -199.9999999999999716, -10.00000000000002665, 6.000000000000000000 ) ) ;
#15326 = CARTESIAN_POINT ( 'NONE',  ( 1.254009781011619751, -13.61532727684435251, 5.487405433548490308 ) ) ;
#15327 = APPLICATION_PROTOCOL_DEFINITION ( 'draft international standard', 'automotive_design', 1998, #13776 ) ;
#15328 =( LENGTH_UNIT ( ) NAMED_UNIT ( * ) SI_UNIT ( .MILLI., .METRE. ) );
#15329 = CARTESIAN_POINT ( 'NONE',  ( 1.861628059977342042, 10.38573835516722355, -6.879051339207178373 ) ) ;
#15330 = DIRECTION ( 'NONE',  ( 0.000000000000000000, 0.000000000000000000, 1.000000000000000000 ) ) ;
#15331 = CARTESIAN_POINT ( 'NONE',  ( 0.3148208552358926493, 8.260375059853341639, 10.97826876274314856 ) ) ;
#15332 = DIRECTION ( 'NONE',  ( 0.9034263296138832500, 0.000000000000000000, 0.4287433579198481337 ) ) ;
#15333 = CARTESIAN_POINT ( 'NONE',  ( 1.845756295923357326, 12.43231724724606835, -0.4783934145702458673 ) ) ;
#15334 = VECTOR ( 'NONE', #5756, 1000.000000000000114 ) ;
#15335 = CARTESIAN_POINT ( 'NONE',  ( 1.342453679581834924, -12.51077660954460136, -7.902645620902585932 ) ) ;
#15336 = ORIENTED_EDGE ( 'NONE', *, *, #4828, .T. ) ;
#15337 = ORIENTED_EDGE ( 'NONE', *, *, #2024, .F. ) ;
#15338 = ORIENTED_EDGE ( 'NONE', *, *, #4741, .T. ) ;
#15339 = ORIENTED_EDGE ( 'NONE', *, *, #1380, .T. ) ;
#15340 = VECTOR ( 'NONE', #6738, 1000.000000000000114 ) ;
#15341 = PLANE ( 'NONE',  #14225 ) ;
#15342 = CARTESIAN_POINT ( 'NONE',  ( 2.117556820461448996, -7.500000000000002665, -15.34001259936770722 ) ) ;
#15343 = EDGE_CURVE ( 'NONE', #15056, #12767, #6210, .T. ) ;
#15344 = ADVANCED_FACE ( 'NONE', ( #7211 ), #2071, .T. ) ;
#15345 = DIRECTION ( 'NONE',  ( 0.000000000000000000, 0.000000000000000000, 1.000000000000000000 ) ) ;
#15346 = CARTESIAN_POINT ( 'NONE',  ( 1.977228804422057840, -7.806978995470733373, 13.27756617201263545 ) ) ;
#15347 = CARTESIAN_POINT ( 'NONE',  ( 1.254255976357671942, -5.487601330835209623, 13.61551404021223455 ) ) ;
#15348 = DIRECTION ( 'NONE',  ( 0.7071067818211348444, 8.659560554583479511E-17, 0.7071067805519601901 ) ) ;
#15349 = CARTESIAN_POINT ( 'NONE',  ( 0.000000000000000000, 0.000000000000000000, -13.00000000000000533 ) ) ;
#15350 = CARTESIAN_POINT ( 'NONE',  ( 5.000000000000006217, -30.00000000000000000, 31.00000000000000000 ) ) ;
#15351 = CARTESIAN_POINT ( 'NONE',  ( 15.00000000000000711, -14.99999999999999645, 3.000000000000000000 ) ) ;
#15352 = EDGE_CURVE ( 'NONE', #10980, #16693, #12439, .T. ) ;
#15353 = CIRCLE ( 'NONE', #2819, 0.5000000000000000000 ) ;
#15354 = ORIENTED_EDGE ( 'NONE', *, *, #14626, .T. ) ;
#15355 = EDGE_LOOP ( 'NONE', ( #16579, #6392, #17160, #17973, #10133 ) ) ;
#15356 = VERTEX_POINT ( 'NONE', #1465 ) ;
#15357 = ORIENTED_EDGE ( 'NONE', *, *, #18112, .F. ) ;
#15358 = CARTESIAN_POINT ( 'NONE',  ( 1.560000000000000053, 0.000000000000000000, 0.000000000000000000 ) ) ;
#15359 = CARTESIAN_POINT ( 'NONE',  ( 16.57778382496167424, 0.01018821665058777630, -0.01092721432668997822 ) ) ;
#15360 = CARTESIAN_POINT ( 'NONE',  ( 3.664313757352979373, 13.97913389346637736, -2.831308606787096949 ) ) ;
#15361 = FACE_OUTER_BOUND ( 'NONE', #15798, .T. ) ;
#15362 = ADVANCED_FACE ( 'NONE', ( #7598 ), #10063, .F. ) ;
#15363 = CARTESIAN_POINT ( 'NONE',  ( 1.846138399168762989, 3.446241763652997836, 11.95493567637851839 ) ) ;
#15364 = ORIENTED_EDGE ( 'NONE', *, *, #14146, .F. ) ;
#15365 = CARTESIAN_POINT ( 'NONE',  ( 16.56782317627811096, -0.0003415813796006971566, 0.009814734722107082768 ) ) ;
#15366 = CIRCLE ( 'NONE', #4071, 14.54644660717763927 ) ;
#15367 = FACE_OUTER_BOUND ( 'NONE', #1451, .T. ) ;
#15368 = EDGE_CURVE ( 'NONE', #6155, #14346, #2651, .T. ) ;
#15369 = ADVANCED_FACE ( 'NONE', ( #11684, #13308 ), #1556, .F. ) ;
#15370 = CARTESIAN_POINT ( 'NONE',  ( -3.431439422792162741, 6.119758975833253345, -11.99999999209397572 ) ) ;
#15371 = CYLINDRICAL_SURFACE ( 'NONE', #2061, 1.000000000000000000 ) ;
#15372 = CARTESIAN_POINT ( 'NONE',  ( 0.3137051932979757485, -8.442169467526770887, -10.83767969834812561 ) ) ;
#15373 = CARTESIAN_POINT ( 'NONE',  ( 2.705023505549862595, -7.115606223895247773, 11.23800170568054568 ) ) ;
#15374 = CARTESIAN_POINT ( 'NONE',  ( 0.3148213771069364175, 0.2297580318216631001, -13.73693585713733967 ) ) ;
#15375 = EDGE_CURVE ( 'NONE', #7136, #4080, #15777, .T. ) ;
#15376 = CARTESIAN_POINT ( 'NONE',  ( 3.950837973638675393, 14.31366178983257242, -2.591948120961654833 ) ) ;
#15377 = ORIENTED_EDGE ( 'NONE', *, *, #10971, .T. ) ;
#15379 = ORIENTED_EDGE ( 'NONE', *, *, #13269, .F. ) ;
#15378 = DIRECTION ( 'NONE',  ( 0.000000000000000000, 0.000000000000000000, 1.000000000000000000 ) ) ;
#15380 = CARTESIAN_POINT ( 'NONE',  ( 0.4862570985993252548, 5.003653737315486794, 12.97920246947881395 ) ) ;
#15381 = EDGE_CURVE ( 'NONE', #4624, #4964, #17615, .T. ) ;
#15382 = AXIS2_PLACEMENT_3D ( 'NONE', #16126, #7436, #168 ) ;
#15383 = VECTOR ( 'NONE', #1599, 1000.000000000000000 ) ;
#15384 = CARTESIAN_POINT ( 'NONE',  ( 3.664313757352971823, 2.831308606787245719, 13.97913389346634183 ) ) ;
#15385 = CARTESIAN_POINT ( 'NONE',  ( 16.56822296793089322, 0.005339139727952925060, 0.008619100080558696197 ) ) ;
#15386 = EDGE_LOOP ( 'NONE', ( #11621, #15916, #3688, #15647 ) ) ;
#15387 = CARTESIAN_POINT ( 'NONE',  ( 2.353870697619111052, 4.720869121224300358, -12.05847592522638934 ) ) ;
#15388 = B_SPLINE_CURVE_WITH_KNOTS ( 'NONE', 3,
 ( #1694, #6097, #17760, #16326, #14883, #3205, #9054, #1796, #7638, #17853, #2189, #15546, #8121 ),
 .UNSPECIFIED., .F., .F.,
 ( 4, 3, 3, 3, 4 ),
 ( 1.897353801849632760E-18, 0.0002299804304191482569, 0.0004599608082120252260, 0.0006467586077648016917, 0.0008336169836825988323 ),
 .UNSPECIFIED. ) ;
#15389 = CARTESIAN_POINT ( 'NONE',  ( -4.525831033740718823, -7.499999999999870326, -13.14978481913338371 ) ) ;
#15390 = ORIENTED_EDGE ( 'NONE', *, *, #5077, .F. ) ;
#15391 = CARTESIAN_POINT ( 'NONE',  ( 1.846138399168762101, -7.646096044339961040, 9.815003036200383946 ) ) ;
#15392 = DIRECTION ( 'NONE',  ( -0.000000000000000000, -0.000000000000000000, -1.000000000000000000 ) ) ;
#15393 = CARTESIAN_POINT ( 'NONE',  ( 0.4862570985993235340, 7.559321496869593204, -11.67702470553357053 ) ) ;
#15394 = CARTESIAN_POINT ( 'NONE',  ( 1.847034903785821136, 10.19974412751574810, -7.126331315909155251 ) ) ;
#15395 = AXIS2_PLACEMENT_3D ( 'NONE', #3847, #15781, #9677 ) ;
#15396 = SURFACE_SIDE_STYLE ('',( #1151 ) ) ;
#15397 = ADVANCED_FACE ( 'NONE', ( #11599 ), #14931, .F. ) ;
#15398 = CARTESIAN_POINT ( 'NONE',  ( 2.002547531651519996, 9.778737580845815458, -7.942910686618064986 ) ) ;
#15399 = LINE ( 'NONE', #5176, #12556 ) ;
#15401 = ORIENTED_EDGE ( 'NONE', *, *, #5210, .T. ) ;
#15400 = CARTESIAN_POINT ( 'NONE',  ( 16.56753206892534891, -0.004368917149004301892, 0.008432171035096367243 ) ) ;
#15402 = CARTESIAN_POINT ( 'NONE',  ( 0.8740764193767940338, -9.070946295054064024, 11.05257066464529281 ) ) ;
#15403 = EDGE_CURVE ( 'NONE', #16657, #11625, #8463, .T. ) ;
#15404 = DIRECTION ( 'NONE',  ( 0.000000000000000000, 0.000000000000000000, 1.000000000000000000 ) ) ;
#15405 = CARTESIAN_POINT ( 'NONE',  ( -5.999999999999998224, 20.00000000000000000, 3.000000000000000000 ) ) ;
#15406 = ORIENTED_EDGE ( 'NONE', *, *, #5540, .T. ) ;
#15407 = AXIS2_PLACEMENT_3D ( 'NONE', #643, #558, #12211 ) ;
#15408 = ORIENTED_EDGE ( 'NONE', *, *, #1544, .T. ) ;
#15409 = DIRECTION ( 'NONE',  ( -0.000000000000000000, -0.000000000000000000, 1.000000000000000000 ) ) ;
#15410 = CARTESIAN_POINT ( 'NONE',  ( 2.747332970342022840, 16.17136872824898575, -2.409922051470736459 ) ) ;
#15411 = VECTOR ( 'NONE', #18672, 1000.000000000000114 ) ;
#15412 = ORIENTED_EDGE ( 'NONE', *, *, #13374, .T. ) ;
#15413 = CARTESIAN_POINT ( 'NONE',  ( 1.342453679581834924, -0.9602753779829698022, -14.76648944001040498 ) ) ;
#15414 = CONICAL_SURFACE ( 'NONE', #2864, 14.54644660717763927, 0.8559913436420816257 ) ;
#15415 = CARTESIAN_POINT ( 'NONE',  ( 16.56822296793089322, 0.007741272030791082788, 0.006547366384935537215 ) ) ;
#15416 = B_SPLINE_CURVE_WITH_KNOTS ( 'NONE', 3,
 ( #12313, #12227, #2184, #3321, #18143, #1808 ),
 .UNSPECIFIED., .F., .F.,
 ( 4, 2, 4 ),
 ( 7.047314121155778821E-19, 0.001657017934712349183, 0.003314035869424697932 ),
 .UNSPECIFIED. ) ;
#15417 = CARTESIAN_POINT ( 'NONE',  ( 1.846613052777651198, -10.26230975746754659, -7.035606253495426898 ) ) ;
#15418 = DIRECTION ( 'NONE',  ( 1.000000000000000000, 0.000000000000000000, 0.000000000000000000 ) ) ;
#15419 = CARTESIAN_POINT ( 'NONE',  ( 2.002547531651519996, 11.75462648437101976, 4.532360870844369671 ) ) ;
#15420 = CARTESIAN_POINT ( 'NONE',  ( 0.3132635586635980074, -13.21855946425834283, -3.740017578711901436 ) ) ;
#15421 = DIRECTION ( 'NONE',  ( 1.000000000000000000, 0.000000000000000000, 0.000000000000000000 ) ) ;
#15422 = ORIENTED_EDGE ( 'NONE', *, *, #17300, .T. ) ;
#15423 = CIRCLE ( 'NONE', #4127, 5.000000000000000888 ) ;
#15424 = AXIS2_PLACEMENT_3D ( 'NONE', #8774, #9056, #7541 ) ;
#15425 = CARTESIAN_POINT ( 'NONE',  ( 1.846138399168762101, -3.446241763652916124, -11.95493567637853971 ) ) ;
#15426 = CARTESIAN_POINT ( 'NONE',  ( 16.56753206892534891, -0.006760771273036217388, -0.006669401563384900512 ) ) ;
#15427 = ADVANCED_FACE ( 'NONE', ( #11882, #26 ), #5844, .T. ) ;
#15428 = EDGE_CURVE ( 'NONE', #9140, #18680, #18237, .T. ) ;
#15429 = EDGE_CURVE ( 'NONE', #4507, #7502, #12349, .T. ) ;
#15430 = CARTESIAN_POINT ( 'NONE',  ( -2.179449471770337432, -4.500000000000000000, -3.000000000000000000 ) ) ;
#15431 = DIRECTION ( 'NONE',  ( 0.7561779333270775005, -0.6322161072786965930, 0.1688126975276491026 ) ) ;
#15432 = ORIENTED_EDGE ( 'NONE', *, *, #16712, .F. ) ;
#15433 = VERTEX_POINT ( 'NONE', #7975 ) ;
#15434 = ORIENTED_EDGE ( 'NONE', *, *, #10347, .T. ) ;
#15435 = ORIENTED_EDGE ( 'NONE', *, *, #893, .F. ) ;
#15436 = DIRECTION ( 'NONE',  ( 0.000000000000000000, 0.000000000000000000, 1.000000000000000000 ) ) ;
#15437 = CARTESIAN_POINT ( 'NONE',  ( -2.816212223827430972, -7.500000000000002665, -15.81854889450412216 ) ) ;
#15438 = CARTESIAN_POINT ( 'NONE',  ( 16.56872352241294521, 0.004907101719995680782, 0.009207754980064214098 ) ) ;
#15439 = CARTESIAN_POINT ( 'NONE',  ( 16.58200780006414732, -0.004047297414158971054, 0.01041078477704053193 ) ) ;
#15440 = CARTESIAN_POINT ( 'NONE',  ( 16.57210152137263393, 0.01453130299868522594, 0.0006600038696346533949 ) ) ;
#15441 = CARTESIAN_POINT ( 'NONE',  ( 0.3720661004400037664, -10.73619472937695640, -8.694226082900707198 ) ) ;
#15442 = CARTESIAN_POINT ( 'NONE',  ( 2.636624412714134280, 2.862162146984768896, 15.80357026013147426 ) ) ;
#15443 = FACE_OUTER_BOUND ( 'NONE', #14309, .T. ) ;
#15444 = EDGE_CURVE ( 'NONE', #17476, #9556, #11027, .T. ) ;
#15445 = ORIENTED_EDGE ( 'NONE', *, *, #3459, .F. ) ;
#15446 = EDGE_CURVE ( 'NONE', #6395, #18405, #8768, .T. ) ;
#15447 = VECTOR ( 'NONE', #16695, 1000.000000000000000 ) ;
#15448 = STYLED_ITEM ( 'NONE', ( #14450 ), #1240 ) ;
#15449 = EDGE_CURVE ( 'NONE', #14774, #2897, #1883, .T. ) ;
#15450 = ORIENTED_EDGE ( 'NONE', *, *, #11458, .T. ) ;
#15451 = ORIENTED_EDGE ( 'NONE', *, *, #9849, .F. ) ;
#15452 = VERTEX_POINT ( 'NONE', #1852 ) ;
#15453 = DIRECTION ( 'NONE',  ( 1.000000000000000000, 0.000000000000000000, -0.000000000000000000 ) ) ;
#15454 = LINE ( 'NONE', #11263, #2879 ) ;
#15455 = DIRECTION ( 'NONE',  ( 0.000000000000000000, 0.000000000000000000, -1.000000000000000000 ) ) ;
#15456 = DIRECTION ( 'NONE',  ( 0.7561779333270775005, 0.6322161072786955938, -0.1688126975276531827 ) ) ;
#15457 = ORIENTED_EDGE ( 'NONE', *, *, #10677, .T. ) ;
#15458 = CARTESIAN_POINT ( 'NONE',  ( 0.3058872367615230181, -8.562166468153638021, -10.75034008168925226 ) ) ;
#15459 = CIRCLE ( 'NONE', #9055, 16.06066017081991149 ) ;
#15460 = CARTESIAN_POINT ( 'NONE',  ( 0.3132642857406501280, 11.41580579227788128, -7.641821025099742926 ) ) ;
#15461 = CARTESIAN_POINT ( 'NONE',  ( -4.196046169205011722, 7.499999999999999112, -16.53685941778014978 ) ) ;
#15462 = CARTESIAN_POINT ( 'NONE',  ( 0.4862570985993235340, -7.559321496869339185, -11.67702470553373750 ) ) ;
#15463 = AXIS2_PLACEMENT_3D ( 'NONE', #16331, #6103, #7735 ) ;
#15464 = TOROIDAL_SURFACE ( 'NONE', #17928, 3.499999999999992450, 0.5000000000000000000 ) ;
#15465 = DIRECTION ( 'NONE',  ( -0.000000000000000000, 1.000000000000000000, 0.000000000000000000 ) ) ;
#15466 = DIRECTION ( 'NONE',  ( -1.000000000000000000, -0.000000000000000000, -0.000000000000000000 ) ) ;
#15467 = CARTESIAN_POINT ( 'NONE',  ( 1.254255976358384705, 12.44256109021893941, -7.789651112956954115 ) ) ;
#15468 = CARTESIAN_POINT ( 'NONE',  ( -194.9999999999999716, 14.99999999999997513, -153.7432847437423789 ) ) ;
#15469 = VERTEX_POINT ( 'NONE', #13872 ) ;
#15470 = AXIS2_PLACEMENT_3D ( 'NONE', #9667, #11386, #15493 ) ;
#15472 = ORIENTED_EDGE ( 'NONE', *, *, #5897, .T. ) ;
#15471 = CYLINDRICAL_SURFACE ( 'NONE', #15170, 2.100000000000000977 ) ;
#15473 = CARTESIAN_POINT ( 'NONE',  ( 0.4754618798421162973, 8.775436892861113947, 10.80499583390515994 ) ) ;
#15474 = VECTOR ( 'NONE', #2599, 1000.000000000000000 ) ;
#15475 = CIRCLE ( 'NONE', #1857, 14.54644660717763927 ) ;
#15476 = ADVANCED_FACE ( 'NONE', ( #7784 ), #18713, .F. ) ;
#15477 = CLOSED_SHELL ( 'NONE', ( #3272, #8111, #6657, #17581, #9377, #12700, #17048, #14573, #10181, #13382, #10873, #7444, #9495, #7933, #4393, #13441, #5284, #18634, #14266, #12514, #4827, #6342, #3245, #11400, #17915, #6784, #8368, #11436, #18732, #14267, #13148, #6512, #6758, #11017, #15953, #10552, #15259, #14845, #1535, #12144, #5078, #7308, #15552, #5612, #16602, #17690, #16205, #1592, #8008, #12149, #5394, #4879, #48, #15220, #5101, #10154, #5761, #16120, #9091, #18834, #13810, #6036, #512, #1557, #17378, #1889, #13387, #3292, #5156, #76, #3356, #6679, #16736, #16391, #3365, #4363, #12028, #16482, #16424, #11123, #3820, #3610, #7037, #3381, #12415, #15023, #6678, #8742, #653, #16778, #2081, #14709, #2468, #13364, #5720, #3699, #12188, #2361, #11382, #15584, #12883, #12387, #4281, #11973, #1492, #3678, #5262, #11315, #15709, #13832, #6799, #18417, #7123, #20, #2977, #14276, #4802, #2052, #12641, #18804, #8148, #8136, #16079, #11991, #2622, #15397, #2944, #11480, #5856, #17985, #5660, #2911 ) ) ;
#15478 = DIRECTION ( 'NONE',  ( -0.000000000000000000, -0.000000000000000000, 1.000000000000000000 ) ) ;
#15479 = ORIENTED_EDGE ( 'NONE', *, *, #13221, .F. ) ;
#15480 = CARTESIAN_POINT ( 'NONE',  ( 1.845756295923360435, -4.296776483139397307, -11.67600463554277468 ) ) ;
#15481 = CARTESIAN_POINT ( 'NONE',  ( -6.500003738482100779, -7.499999999999348965, -12.10028435765593890 ) ) ;
#15482 = ORIENTED_EDGE ( 'NONE', *, *, #4981, .F. ) ;
#15483 = CARTESIAN_POINT ( 'NONE',  ( 0.8740764193767940338, -9.070946295054064024, 11.05257066464529281 ) ) ;
#15484 = DIRECTION ( 'NONE',  ( -1.000000000000000000, 0.000000000000000000, 0.000000000000000000 ) ) ;
#15485 = CARTESIAN_POINT ( 'NONE',  ( 1.321128355694181398E-14, -8.013167318348353163, 25.01316734529530095 ) ) ;
#15486 = CARTESIAN_POINT ( 'NONE',  ( 1.847461586945727152, 10.04711372545055781, -7.341074796295831817 ) ) ;
#15487 = DIRECTION ( 'NONE',  ( 1.182917971378669349E-16, -0.2588190451025214611, 0.9659258262890679791 ) ) ;
#15488 = EDGE_CURVE ( 'NONE', #18705, #13316, #9487, .T. ) ;
#15489 = B_SPLINE_CURVE_WITH_KNOTS ( 'NONE', 3,
 ( #12273, #18104, #5003, #16670 ),
 .UNSPECIFIED., .F., .F.,
 ( 4, 4 ),
 ( 1.117853977359352840E-16, 0.002004993803842554205 ),
 .UNSPECIFIED. ) ;
#15490 =( NAMED_UNIT ( * ) SI_UNIT ( $, .STERADIAN. ) SOLID_ANGLE_UNIT ( ) );
#15491 = CARTESIAN_POINT ( 'NONE',  ( 3.950837973638675393, -13.10350451991845055, 6.316429227969417859 ) ) ;
#15492 = CARTESIAN_POINT ( 'NONE',  ( -30.00000000000000355, -12.50000000000000178, -0.5000000000000000000 ) ) ;
#15494 = ORIENTED_EDGE ( 'NONE', *, *, #10473, .T. ) ;
#15493 = DIRECTION ( 'NONE',  ( 1.000000000000000000, 0.000000000000000000, 0.000000000000000000 ) ) ;
#15495 = CARTESIAN_POINT ( 'NONE',  ( 0.3095370825347224519, -10.84046130709052491, -8.444334731364122604 ) ) ;
#15496 = VERTEX_POINT ( 'NONE', #10647 ) ;
#15497 = AXIS2_PLACEMENT_3D ( 'NONE', #16772, #9130, #4736 ) ;
#15498 = CARTESIAN_POINT ( 'NONE',  ( 1.342453679581834924, -0.9602753779829698022, -14.76648944001040498 ) ) ;
#15499 = CARTESIAN_POINT ( 'NONE',  ( 1.861628059977342486, 4.358833901513207820, -11.66985327793194216 ) ) ;
#15500 = VERTEX_POINT ( 'NONE', #7692 ) ;
#15501 = VERTEX_POINT ( 'NONE', #10547 ) ;
#15502 = CARTESIAN_POINT ( 'NONE',  ( 0.000000000000000000, 0.000000000000000000, -2.000000000000000000 ) ) ;
#15503 = CARTESIAN_POINT ( 'NONE',  ( 0.3308579732647032867, 10.76782854710826776, 8.558831104906948539 ) ) ;
#15504 = EDGE_LOOP ( 'NONE', ( #2851, #13271, #9307, #1952, #13410 ) ) ;
#15505 = CARTESIAN_POINT ( 'NONE',  ( 3.950837973638676281, -10.05648675950133963, 10.51028938476214059 ) ) ;
#15506 = CARTESIAN_POINT ( 'NONE',  ( 1.861706995891664773, 10.38589138506426934, 6.878962591851789377 ) ) ;
#15507 = CARTESIAN_POINT ( 'NONE',  ( 0.3058872367615226295, -11.46514199369363318, 7.578326039752564469 ) ) ;
#15508 = DIRECTION ( 'NONE',  ( 0.000000000000000000, 0.000000000000000000, 1.000000000000000000 ) ) ;
#15509 = FACE_OUTER_BOUND ( 'NONE', #9648, .T. ) ;
#15510 = CARTESIAN_POINT ( 'NONE',  ( 1.847247051441591292, 7.177495230324704600, 10.16425585218603267 ) ) ;
#15511 = APPLICATION_PROTOCOL_DEFINITION ( 'draft international standard', 'automotive_design', 1998, #6695 ) ;
#15512 = B_SPLINE_CURVE_WITH_KNOTS ( 'NONE', 3,
 ( #13425, #5866, #340, #11708, #4547, #10371, #16201 ),
 .UNSPECIFIED., .F., .F.,
 ( 4, 3, 4 ),
 ( 1.843143693225357538E-18, 0.0002299804304191480943, 0.0004168119862255878537 ),
 .UNSPECIFIED. ) ;
#15513 = CARTESIAN_POINT ( 'NONE',  ( 16.56822296793089322, 0.006547366384936635295, 0.007741272030791194678 ) ) ;
#15514 = ADVANCED_FACE ( 'NONE', ( #3265 ), #9396, .T. ) ;
#15515 = CARTESIAN_POINT ( 'NONE',  ( 2.636624412715999011, 2.161493821598055920, -15.91454522070273647 ) ) ;
#15516 = DIRECTION ( 'NONE',  ( -0.000000000000000000, 1.000000000000000000, -0.000000000000000000 ) ) ;
#15517 = CARTESIAN_POINT ( 'NONE',  ( 0.3170788640506440603, 4.100430649997962362, 13.11595226728159425 ) ) ;
#15518 = CARTESIAN_POINT ( 'NONE',  ( 2.002547531651519996, 12.57989064830759496, -0.6781519942172177240 ) ) ;
#15519 = CARTESIAN_POINT ( 'NONE',  ( 2.002547531651519996, 7.942910686618313676, -9.778737580845612953 ) ) ;
#15520 = VERTEX_POINT ( 'NONE', #6627 ) ;
#15521 = EDGE_LOOP ( 'NONE', ( #17730, #2574, #12030, #14054 ) ) ;
#15522 = VERTEX_POINT ( 'NONE', #6244 ) ;
#15523 = ORIENTED_EDGE ( 'NONE', *, *, #15897, .T. ) ;
#15524 = B_SPLINE_CURVE_WITH_KNOTS ( 'NONE', 3,
 ( #10372, #10083, #15912, #10273, #8647, #14570 ),
 .UNSPECIFIED., .F., .F.,
 ( 4, 2, 4 ),
 ( 3.527508043940425264E-17, 0.0001825746017570591031, 0.0003651492035140829697 ),
 .UNSPECIFIED. ) ;
#15525 = CARTESIAN_POINT ( 'NONE',  ( 0.3307726912345187453, 0.5948952607472642873, 13.74203354050372461 ) ) ;
#15526 = CARTESIAN_POINT ( 'NONE',  ( 0.3939822652208163078, 4.930560016699244485, -12.90851734139301499 ) ) ;
#15527 = EDGE_CURVE ( 'NONE', #16287, #13667, #16480, .T. ) ;
#15528 = CARTESIAN_POINT ( 'NONE',  ( 16.56753206892534891, -0.004368917149005395635, -0.008432171035096433162 ) ) ;
#15529 = DIRECTION ( 'NONE',  ( -0.000000000000000000, -0.000000000000000000, 1.000000000000000000 ) ) ;
#15530 =( LENGTH_UNIT ( ) NAMED_UNIT ( * ) SI_UNIT ( .MILLI., .METRE. ) );
#15531 = CARTESIAN_POINT ( 'NONE',  ( 2.002547531651519996, -4.532360870844247991, -11.75462648437106417 ) ) ;
#15532 = LINE ( 'NONE', #5669, #15199 ) ;
#15533 = MECHANICAL_DESIGN_GEOMETRIC_PRESENTATION_REPRESENTATION (  '', ( #14315 ), #892 ) ;
#15534 = CIRCLE ( 'NONE', #8075, 5.000000000000004441 ) ;
#15535 = CARTESIAN_POINT ( 'NONE',  ( 16.56753206892534891, 0.009369540855502130061, 0.001549402974393180796 ) ) ;
#15536 = DIRECTION ( 'NONE',  ( 0.000000000000000000, 0.000000000000000000, 1.000000000000000000 ) ) ;
#15537 = ORIENTED_EDGE ( 'NONE', *, *, #1658, .T. ) ;
#15538 =( BOUNDED_SURFACE ( )  B_SPLINE_SURFACE ( 3, 1, ( 
 ( #1028, #3996 ),
 ( #2822, #10007 ),
 ( #6869, #14224 ),
 ( #18699, #14401 ) ),
 .UNSPECIFIED., .F., .F., .T. ) 
 B_SPLINE_SURFACE_WITH_KNOTS ( ( 4, 4 ),
 ( 2, 2 ),
 ( 0.000000000000000000, 1.000000000000000000 ),
 ( 0.000000000000000000, 1.000000000000000000 ),
 .UNSPECIFIED. ) 
 GEOMETRIC_REPRESENTATION_ITEM ( )  RATIONAL_B_SPLINE_SURFACE ( (
 ( 1.000000000000000000, 1.000000000000000000),
 ( 0.9933953342250438912, 0.8357391271907739227),
 ( 0.9933953342250438912, 0.8357391271907739227),
 ( 1.000000000000000000, 1.000000000000000000) ) ) 
 REPRESENTATION_ITEM ( '' )  SURFACE ( )  );
#15539 = ORIENTED_EDGE ( 'NONE', *, *, #1073, .T. ) ;
#15540 = VECTOR ( 'NONE', #333, 1000.000000000000114 ) ;
#15541 = ORIENTED_EDGE ( 'NONE', *, *, #8735, .T. ) ;
#15542 = ORIENTED_EDGE ( 'NONE', *, *, #8507, .F. ) ;
#15543 = B_SPLINE_CURVE_WITH_KNOTS ( 'NONE', 3,
 ( #4760, #2916, #18893, #13161, #8775, #14688 ),
 .UNSPECIFIED., .F., .F.,
 ( 4, 2, 4 ),
 ( 0.000000000000000000, 0.001657017934710630505, 0.003314035869421261011 ),
 .UNSPECIFIED. ) ;
#15544 = CARTESIAN_POINT ( 'NONE',  ( 1.846613052777651198, 3.520031056876471887, -11.93415846513958023 ) ) ;
#15545 = CARTESIAN_POINT ( 'NONE',  ( 1.846524061778019421, -7.023652644192194927, -10.27028962889604813 ) ) ;
#15546 = CARTESIAN_POINT ( 'NONE',  ( 1.846524061778019199, 12.43723828841088341, 0.3544704288992919228 ) ) ;
#15547 = CARTESIAN_POINT ( 'NONE',  ( 0.3720661004400037664, -8.694226082900666341, 10.73619472937699015 ) ) ;
#15548 = CARTESIAN_POINT ( 'NONE',  ( 1.977228804421389485, 13.27756617201186096, 7.806978995470745808 ) ) ;
#15549 = ORIENTED_EDGE ( 'NONE', *, *, #6574, .T. ) ;
#15550 = FACE_OUTER_BOUND ( 'NONE', #6135, .T. ) ;
#15551 = EDGE_CURVE ( 'NONE', #14405, #17750, #17011, .T. ) ;
#15552 = ADVANCED_FACE ( 'NONE', ( #16381 ), #3717, .F. ) ;
#15553 = CARTESIAN_POINT ( 'NONE',  ( 1.846613052777650310, -11.93415846513959444, -3.520031056876430142 ) ) ;
#15554 = CARTESIAN_POINT ( 'NONE',  ( 6.538348415311013184, 7.500000000000000000, -12.00000000000000000 ) ) ;
#15555 = CARTESIAN_POINT ( 'NONE',  ( 1.845755665166724846, -6.920419570228271589, -10.33920510797150882 ) ) ;
#15556 = CARTESIAN_POINT ( 'NONE',  ( 0.4384471787762813100, -8.732395932355604629, -10.76632603192796722 ) ) ;
#15557 = CARTESIAN_POINT ( 'NONE',  ( 0.3132642857406530146, 13.21852905223344088, -3.740125687984594993 ) ) ;
#15558 = CARTESIAN_POINT ( 'NONE',  ( 0.3137051932979792457, 4.679953077377670745, -12.91601973349265720 ) ) ;
#15559 = DIRECTION ( 'NONE',  ( -1.000000000000000000, 0.000000000000000000, 0.000000000000000000 ) ) ;
#15560 = VERTEX_POINT ( 'NONE', #12263 ) ;
#15562 = ORIENTED_EDGE ( 'NONE', *, *, #8671, .T. ) ;
#15561 = DIRECTION ( 'NONE',  ( -1.000000000000000000, -0.000000000000000000, -0.000000000000000000 ) ) ;
#15563 = CARTESIAN_POINT ( 'NONE',  ( 2.002547531651521773, 9.778737580845699995, 7.942910686618207983 ) ) ;
#15564 = CARTESIAN_POINT ( 'NONE',  ( 16.57605080000000086, 0.000000000000000000, 0.000000000000000000 ) ) ;
#15565 = ORIENTED_EDGE ( 'NONE', *, *, #13893, .T. ) ;
#15566 = CARTESIAN_POINT ( 'NONE',  ( -4.999999999999995559, -30.00000000000000000, 6.000000000000000000 ) ) ;
#15567 = CARTESIAN_POINT ( 'NONE',  ( -30.00000000000000355, -12.50000000000000178, 6.000000000000000000 ) ) ;
#15568 = CARTESIAN_POINT ( 'NONE',  ( 3.074695600507118431, 2.772091048739504959, -15.30693405987805811 ) ) ;
#15569 = VERTEX_POINT ( 'NONE', #18093 ) ;
#15570 = CARTESIAN_POINT ( 'NONE',  ( 1.847412631396503357, -7.348689888531914072, 10.04119192206683664 ) ) ;
#15571 = CARTESIAN_POINT ( 'NONE',  ( 0.8740764193766769052, -13.83508774436000088, 3.609949042658186169 ) ) ;
#15572 = CARTESIAN_POINT ( 'NONE',  ( 2.636624412715138366, -11.10302021257964888, 11.60464335004044223 ) ) ;
#15573 =( BOUNDED_SURFACE ( )  B_SPLINE_SURFACE ( 3, 1, ( 
 ( #16096, #15987 ),
 ( #7218, #18859 ),
 ( #33, #11604 ),
 ( #11795, #2881 ) ),
 .UNSPECIFIED., .F., .F., .F. ) 
 B_SPLINE_SURFACE_WITH_KNOTS ( ( 4, 4 ),
 ( 2, 2 ),
 ( 0.000000000000000000, 1.000000000000000000 ),
 ( 0.000000000000000000, 1.000000000000000000 ),
 .UNSPECIFIED. ) 
 GEOMETRIC_REPRESENTATION_ITEM ( )  RATIONAL_B_SPLINE_SURFACE ( (
 ( 1.000000000000000000, 1.000000000000000000),
 ( 0.7792777138730158093, 0.9689936506012928330),
 ( 0.7792777138730158093, 0.9689936506012928330),
 ( 1.000000000000000000, 1.000000000000000000) ) ) 
 REPRESENTATION_ITEM ( '' )  SURFACE ( )  );
#15574 = FACE_OUTER_BOUND ( 'NONE', #12983, .T. ) ;
#15575 = CARTESIAN_POINT ( 'NONE',  ( 2.002547531651519996, 7.942910686618173344, 9.778737580845726640 ) ) ;
#15576 = EDGE_CURVE ( 'NONE', #4785, #381, #8705, .T. ) ;
#15577 = EDGE_CURVE ( 'NONE', #846, #5396, #8249, .T. ) ;
#15578 = SHAPE_REPRESENTATION_RELATIONSHIP ( 'NONE' , 'NONE' ,  #14244, #6229 ) ;
#15579 = CARTESIAN_POINT ( 'NONE',  ( 0.4862570985993235340, 7.559321496869593204, -11.67702470553357053 ) ) ;
#15580 = B_SPLINE_CURVE_WITH_KNOTS ( 'NONE', 3,
 ( #688, #402, #6521, #10435 ),
 .UNSPECIFIED., .F., .F.,
 ( 4, 4 ),
 ( 2.851299179213411365E-16, 0.002004993803842618823 ),
 .UNSPECIFIED. ) ;
#15582 = ORIENTED_EDGE ( 'NONE', *, *, #4041, .F. ) ;
#15581 = DIRECTION ( 'NONE',  ( 0.000000000000000000, 0.000000000000000000, 1.000000000000000000 ) ) ;
#15583 = CARTESIAN_POINT ( 'NONE',  ( 1.977228804423455610, 11.52787183731216381, -10.21522664410554881 ) ) ;
#15584 = ADVANCED_FACE ( 'NONE', ( #15674 ), #7645, .F. ) ;
#15585 = LINE ( 'NONE', #4314, #4646 ) ;
#15586 = CARTESIAN_POINT ( 'NONE',  ( 2.750000000000000000, 3.306546357697853733E-16, -2.700000000000000178 ) ) ;
#15587 = VERTEX_POINT ( 'NONE', #13970 ) ;
#15588 = CARTESIAN_POINT ( 'NONE',  ( 8.522092701127531811, -4.388629235579615262, 5.397361180353127175 ) ) ;
#15589 = CARTESIAN_POINT ( 'NONE',  ( 2.179449471770337432, -4.500000000000000000, -3.000000000000000000 ) ) ;
#15590 = VERTEX_POINT ( 'NONE', #14152 ) ;
#15591 = CARTESIAN_POINT ( 'NONE',  ( 3.950837973638668288, 0.000000000000000000, 0.000000000000000000 ) ) ;
#15592 = CARTESIAN_POINT ( 'NONE',  ( 1.254009781011991898, 3.563484327698415388, -14.24044713813362151 ) ) ;
#15593 = CONICAL_SURFACE ( 'NONE', #18055, 1732.050807568857181, 1.047197551196592746 ) ;
#15594 = PRODUCT_RELATED_PRODUCT_CATEGORY ( 'part', '', ( #12278 ) ) ;
#15595 = CARTESIAN_POINT ( 'NONE',  ( -199.9999999999999716, -10.00000000000002665, 3.000000000000000000 ) ) ;
#15596 = EDGE_CURVE ( 'NONE', #4800, #13818, #14423, .T. ) ;
#15597 = CARTESIAN_POINT ( 'NONE',  ( 0.3137051932979792457, -10.83767969834809008, 8.442169467526815296 ) ) ;
#15598 = DIRECTION ( 'NONE',  ( 0.000000000000000000, 0.000000000000000000, 1.000000000000000000 ) ) ;
#15599 = ADVANCED_FACE ( 'NONE', ( #9944 ), #11530, .F. ) ;
#15600 = ADVANCED_FACE ( 'NONE', ( #17116, #1156, #8337 ), #18638, .F. ) ;
#15601 = SHAPE_DEFINITION_REPRESENTATION ( #5829, #6437 ) ;
#15602 = CARTESIAN_POINT ( 'NONE',  ( -32.49999999999999289, -12.50000000000000178, 3.000000000000000000 ) ) ;
#15603 = DIRECTION ( 'NONE',  ( -1.000000000000000000, -1.040834085586084257E-15, 0.000000000000000000 ) ) ;
#15604 = CARTESIAN_POINT ( 'NONE',  ( 0.4862570985993235340, -10.79774104611379215, 8.769551628660700260 ) ) ;
#15605 = CARTESIAN_POINT ( 'NONE',  ( -194.9999999999999716, -15.00000000000003020, 3.000000000000002665 ) ) ;
#15606 = DIRECTION ( 'NONE',  ( 0.000000000000000000, 0.000000000000000000, 1.000000000000000000 ) ) ;
#15607 = SURFACE_STYLE_FILL_AREA ( #5560 ) ;
#15608 = ORIENTED_EDGE ( 'NONE', *, *, #14147, .T. ) ;
#15609 = EDGE_CURVE ( 'NONE', #4997, #4745, #18365, .T. ) ;
#15610 = VERTEX_POINT ( 'NONE', #5538 ) ;
#15611 = EDGE_LOOP ( 'NONE', ( #12089, #11073, #13604, #971 ) ) ;
#15612 = CIRCLE ( 'NONE', #12572, 16.06066017081991149 ) ;
#15613 = ORIENTED_EDGE ( 'NONE', *, *, #4755, .F. ) ;
#15614 = CARTESIAN_POINT ( 'NONE',  ( -194.9999999999999716, -45.00000000000003553, 0.000000000000000000 ) ) ;
#15615 = FACE_OUTER_BOUND ( 'NONE', #6581, .T. ) ;
#15616 = CARTESIAN_POINT ( 'NONE',  ( -5.000000000000000888, 17.00000000000000000, 7.000000000000000000 ) ) ;
#15617 = LINE ( 'NONE', #7032, #18474 ) ;
#15618 = CARTESIAN_POINT ( 'NONE',  ( 1.846138399168762101, 9.815003036200520725, -7.646096044339786069 ) ) ;
#15619 = DIRECTION ( 'NONE',  ( -0.000000000000000000, -0.000000000000000000, 1.000000000000000000 ) ) ;
#15620 = AXIS2_PLACEMENT_3D ( 'NONE', #7607, #16098, #6063 ) ;
#15621 = CARTESIAN_POINT ( 'NONE',  ( 16.56782317627811096, 0.009439921864426468329, 0.002708056627497651414 ) ) ;
#15622 = CARTESIAN_POINT ( 'NONE',  ( 16.56872352241294521, -0.009207754980064163791, 0.004907101719995779661 ) ) ;
#15623 = ORIENTED_EDGE ( 'NONE', *, *, #8017, .T. ) ;
#15624 = ORIENTED_EDGE ( 'NONE', *, *, #5264, .T. ) ;
#15625 = EDGE_CURVE ( 'NONE', #4817, #3568, #6721, .T. ) ;
#15626 = EDGE_LOOP ( 'NONE', ( #481, #10338, #1161, #13365, #14207, #9603 ) ) ;
#15627 = ORIENTED_EDGE ( 'NONE', *, *, #7311, .T. ) ;
#15628 = ORIENTED_EDGE ( 'NONE', *, *, #12248, .T. ) ;
#15629 = DIRECTION ( 'NONE',  ( -0.000000000000000000, -1.000000000000000000, -0.000000000000000000 ) ) ;
#15630 = CARTESIAN_POINT ( 'NONE',  ( 3.950837973638677170, -14.31366178983255466, 2.591948120961746760 ) ) ;
#15631 = CARTESIAN_POINT ( 'NONE',  ( 1.847034903785821136, 10.19974412751574810, -7.126331315909155251 ) ) ;
#15632 = DIRECTION ( 'NONE',  ( 1.000000000000000000, 0.000000000000000000, -0.000000000000000000 ) ) ;
#15633 = ORIENTED_EDGE ( 'NONE', *, *, #2848, .T. ) ;
#15634 = CARTESIAN_POINT ( 'NONE',  ( 16.56782317627811096, -0.0003415813796006971566, 0.009814734722107082768 ) ) ;
#15635 = CARTESIAN_POINT ( 'NONE',  ( 1.861628059977342931, -12.00316790821103652, 3.332996951203584413 ) ) ;
#15636 = B_SPLINE_CURVE_WITH_KNOTS ( 'NONE', 3,
 ( #5825, #4699, #305, #15009, #3242, #6133 ),
 .UNSPECIFIED., .F., .F.,
 ( 4, 2, 4 ),
 ( 4.083989690778167730E-17, 0.0002014099069817300042, 0.0004028198139634191341 ),
 .UNSPECIFIED. ) ;
#15637 = CARTESIAN_POINT ( 'NONE',  ( 6.259160902251540648, 7.500000000000127898, -12.42139992667815562 ) ) ;
#15638 = DIRECTION ( 'NONE',  ( -0.000000000000000000, 0.5000000000000004441, 0.8660254037844383745 ) ) ;
#15639 = AXIS2_PLACEMENT_3D ( 'NONE', #18472, #11132, #3859 ) ;
#15640 = CARTESIAN_POINT ( 'NONE',  ( 16.56872352241294521, 0.007240717549633888563, 0.007512283835804339609 ) ) ;
#15641 = CARTESIAN_POINT ( 'NONE',  ( 2.747332970342022840, 14.63517873738947195, 7.289199830147158998 ) ) ;
#15642 = DIRECTION ( 'NONE',  ( -1.000000000000000000, -1.601283208593975514E-16, 0.000000000000000000 ) ) ;
#15643 =( BOUNDED_SURFACE ( )  B_SPLINE_SURFACE ( 3, 1, ( 
 ( #1097, #12761 ),
 ( #18584, #5490 ),
 ( #17154, #4066 ),
 ( #9884, #2991 ) ),
 .UNSPECIFIED., .F., .F., .T. ) 
 B_SPLINE_SURFACE_WITH_KNOTS ( ( 4, 4 ),
 ( 2, 2 ),
 ( 0.000000000000000000, 1.000000000000000000 ),
 ( 0.000000000000000000, 1.000000000000000000 ),
 .UNSPECIFIED. ) 
 GEOMETRIC_REPRESENTATION_ITEM ( )  RATIONAL_B_SPLINE_SURFACE ( (
 ( 1.000000000000000000, 1.000000000000000000),
 ( 0.7792777138730158093, 0.9689936506012928330),
 ( 0.7792777138730158093, 0.9689936506012928330),
 ( 1.000000000000000000, 1.000000000000000000) ) ) 
 REPRESENTATION_ITEM ( '' )  SURFACE ( )  );
#15644 = LINE ( 'NONE', #18801, #3293 ) ;
#15645 = VERTEX_POINT ( 'NONE', #11114 ) ;
#15647 = ORIENTED_EDGE ( 'NONE', *, *, #3890, .F. ) ;
#15646 = CARTESIAN_POINT ( 'NONE',  ( 0.3137051932979792457, 7.698472063774471685, 11.37800749014133928 ) ) ;
#15648 = FACE_OUTER_BOUND ( 'NONE', #7684, .T. ) ;
#15649 = EDGE_CURVE ( 'NONE', #4326, #16313, #3839, .T. ) ;
#15650 = EDGE_CURVE ( 'NONE', #11605, #12470, #16938, .T. ) ;
#15651 = EDGE_CURVE ( 'NONE', #15433, #8892, #13276, .T. ) ;
#15652 = CARTESIAN_POINT ( 'NONE',  ( 1.847247051441591514, -0.1676840720646167182, 12.44188156437794213 ) ) ;
#15653 = B_SPLINE_CURVE_WITH_KNOTS ( 'NONE', 3,
 ( #7247, #2815, #13155, #10098 ),
 .UNSPECIFIED., .F., .F.,
 ( 4, 4 ),
 ( 0.000000000000000000, 0.002004993803842804005 ),
 .UNSPECIFIED. ) ;
#15654 = AXIS2_PLACEMENT_3D ( 'NONE', #8796, #7081, #14616 ) ;
#15655 = ORIENTED_EDGE ( 'NONE', *, *, #4826, .F. ) ;
#15656 = CARTESIAN_POINT ( 'NONE',  ( 3.950837973638676281, -12.81214529934970336, -6.888253895133431115 ) ) ;
#15657 = CARTESIAN_POINT ( 'NONE',  ( 1.847380140988739150, -12.44273713935591097, 0.1101766933248207875 ) ) ;
#15658 = CARTESIAN_POINT ( 'NONE',  ( -66.35602477868049220, -15.00000000000001066, 3.000000000000002665 ) ) ;
#15659 = DIRECTION ( 'NONE',  ( 0.7561779333270775005, 0.4122479608995740508, -0.5081796452863232005 ) ) ;
#15660 = ORIENTED_EDGE ( 'NONE', *, *, #13912, .T. ) ;
#15661 = CARTESIAN_POINT ( 'NONE',  ( 3.950837973638676281, -14.41405733518061716, 1.958075594453740687 ) ) ;
#15662 = DIRECTION ( 'NONE',  ( -1.000000000000000000, -0.000000000000000000, -0.000000000000000000 ) ) ;
#15663 = DIRECTION ( 'NONE',  ( 0.000000000000000000, 0.000000000000000000, 1.000000000000000000 ) ) ;
#15664 = CARTESIAN_POINT ( 'NONE',  ( 3.950837973638677170, -1.958075594453692503, -14.41405733518062959 ) ) ;
#15665 = EDGE_CURVE ( 'NONE', #17143, #15164, #8941, .T. ) ;
#15666 = DIRECTION ( 'NONE',  ( 0.000000000000000000, 0.000000000000000000, 1.000000000000000000 ) ) ;
#15667 = CARTESIAN_POINT ( 'NONE',  ( 16.56872352241294521, 0.004564908236400220913, 0.009382111268606271176 ) ) ;
#15668 = VECTOR ( 'NONE', #17171, 1000.000000000000000 ) ;
#15669 =( GEOMETRIC_REPRESENTATION_CONTEXT ( 3 ) GLOBAL_UNCERTAINTY_ASSIGNED_CONTEXT ( ( #8434 ) ) GLOBAL_UNIT_ASSIGNED_CONTEXT ( ( #2113, #18067, #3432 ) ) REPRESENTATION_CONTEXT ( 'NONE', 'WORKASPACE' ) );
#15670 = ORIENTED_EDGE ( 'NONE', *, *, #4025, .F. ) ;
#15671 = FACE_BOUND ( 'NONE', #2550, .T. ) ;
#15673 = ORIENTED_EDGE ( 'NONE', *, *, #5897, .F. ) ;
#15672 = DIRECTION ( 'NONE',  ( -1.000000000000000000, 0.000000000000000000, -0.000000000000000000 ) ) ;
#15674 = FACE_OUTER_BOUND ( 'NONE', #16715, .T. ) ;
#15675 = DIRECTION ( 'NONE',  ( 0.000000000000000000, -0.000000000000000000, -1.000000000000000000 ) ) ;
#15676 = VERTEX_POINT ( 'NONE', #11862 ) ;
#15677 = CARTESIAN_POINT ( 'NONE',  ( 3.377929128793395908, -12.84367544717939680, 5.536064832134110603 ) ) ;
#15678 = EDGE_CURVE ( 'NONE', #15103, #4379, #12731, .T. ) ;
#15679 = CARTESIAN_POINT ( 'NONE',  ( 16.56872352241294521, -0.007240717549633941472, -0.007512283835804289302 ) ) ;
#15680 =( BOUNDED_SURFACE ( )  B_SPLINE_SURFACE ( 3, 1, ( 
 ( #14406, #14869 ),
 ( #14324, #10574 ),
 ( #2650, #7623 ),
 ( #16414, #12104 ) ),
 .UNSPECIFIED., .F., .F., .T. ) 
 B_SPLINE_SURFACE_WITH_KNOTS ( ( 4, 4 ),
 ( 2, 2 ),
 ( 0.000000000000000000, 1.000000000000000000 ),
 ( 0.000000000000000000, 1.000000000000000000 ),
 .UNSPECIFIED. ) 
 GEOMETRIC_REPRESENTATION_ITEM ( )  RATIONAL_B_SPLINE_SURFACE ( (
 ( 1.000000000000000000, 1.000000000000000000),
 ( 0.9933953342250436691, 0.8357391271907733676),
 ( 0.9933953342250436691, 0.8357391271907733676),
 ( 1.000000000000000000, 1.000000000000000000) ) ) 
 REPRESENTATION_ITEM ( '' )  SURFACE ( )  );
#15681 =( BOUNDED_SURFACE ( )  B_SPLINE_SURFACE ( 3, 1, ( 
 ( #9245, #6291 ),
 ( #12019, #3406 ),
 ( #4856, #10590 ),
 ( #4661, #1989 ) ),
 .UNSPECIFIED., .F., .F., .T. ) 
 B_SPLINE_SURFACE_WITH_KNOTS ( ( 4, 4 ),
 ( 2, 2 ),
 ( 0.000000000000000000, 1.000000000000000000 ),
 ( 0.000000000000000000, 1.000000000000000000 ),
 .UNSPECIFIED. ) 
 GEOMETRIC_REPRESENTATION_ITEM ( )  RATIONAL_B_SPLINE_SURFACE ( (
 ( 1.000000000000000000, 1.000000000000000000),
 ( 0.9933953342250436691, 0.8357391271907733676),
 ( 0.9933953342250436691, 0.8357391271907733676),
 ( 1.000000000000000000, 1.000000000000000000) ) ) 
 REPRESENTATION_ITEM ( '' )  SURFACE ( )  );
#15682 = ORIENTED_EDGE ( 'NONE', *, *, #15320, .T. ) ;
#15683 = CARTESIAN_POINT ( 'NONE',  ( 0.3148208552358953138, -8.260375059853256374, -10.97826876274321428 ) ) ;
#15684 = CARTESIAN_POINT ( 'NONE',  ( 2.123976203522053297, 1.531817366691969884, -15.54801196254785189 ) ) ;
#15685 = AXIS2_PLACEMENT_3D ( 'NONE', #12140, #6114, #10507 ) ;
#15686 = LINE ( 'NONE', #14162, #7624 ) ;
#15687 = CARTESIAN_POINT ( 'NONE',  ( 5.000000000000004441, -27.00000000000000000, 26.00000000000000000 ) ) ;
#15688 = CARTESIAN_POINT ( 'NONE',  ( 2.002547531651519996, 12.17374746633578475, 3.242439124566693476 ) ) ;
#15689 = UNCERTAINTY_MEASURE_WITH_UNIT (LENGTH_MEASURE( 1.000000000000000082E-05 ), #6212, 'distance_accuracy_value', 'NONE');
#15690 = EDGE_CURVE ( 'NONE', #17676, #2099, #18731, .T. ) ;
#15691 = ORIENTED_EDGE ( 'NONE', *, *, #3302, .T. ) ;
#15692 = CONTEXT_DEPENDENT_SHAPE_REPRESENTATION ( #2299, #7869 ) ;
#15693 = DIRECTION ( 'NONE',  ( -0.000000000000000000, -0.000000000000000000, -1.000000000000000000 ) ) ;
#15694 = CARTESIAN_POINT ( 'NONE',  ( 16.56872352241294521, 0.009207754980064196751, -0.004907101719995712874 ) ) ;
#15695 = CARTESIAN_POINT ( 'NONE',  ( 1.846955891736119737, 0.2634721419535199782, 12.44001089941741256 ) ) ;
#15696 = CARTESIAN_POINT ( 'NONE',  ( 1.847372867223028070, 3.744745203533978106, 11.86627781945709792 ) ) ;
#15697 = CARTESIAN_POINT ( 'NONE',  ( 0.000000000000000000, 0.000000000000000000, 7.000000000000000000 ) ) ;
#15698 = B_SPLINE_CURVE_WITH_KNOTS ( 'NONE', 3,
 ( #1068, #18561, #2683, #11312, #17128, #9851 ),
 .UNSPECIFIED., .F., .F.,
 ( 4, 2, 4 ),
 ( 0.000000000000000000, 0.0001828790815886955387, 0.0003657581631773888006 ),
 .UNSPECIFIED. ) ;
#15699 = VERTEX_POINT ( 'NONE', #16160 ) ;
#15700 = CARTESIAN_POINT ( 'NONE',  ( 0.3148208552358927048, 10.97826876274324270, -8.260375059853219071 ) ) ;
#15701 = CARTESIAN_POINT ( 'NONE',  ( 16.58200780006414732, -0.01080144354108990290, 0.002844973367390998473 ) ) ;
#15702 = ORIENTED_EDGE ( 'NONE', *, *, #4932, .T. ) ;
#15703 = CIRCLE ( 'NONE', #17540, 3.499999999999992895 ) ;
#15704 = ORIENTED_EDGE ( 'NONE', *, *, #4097, .T. ) ;
#15705 = ORIENTED_EDGE ( 'NONE', *, *, #13789, .T. ) ;
#15706 = DIRECTION ( 'NONE',  ( 0.000000000000000000, 0.000000000000000000, 1.000000000000000000 ) ) ;
#15707 = ORIENTED_EDGE ( 'NONE', *, *, #2442, .F. ) ;
#15708 = CARTESIAN_POINT ( 'NONE',  ( 2.002547531651519996, 0.6781519942173496185, -12.57989064830758785 ) ) ;
#15709 = ADVANCED_FACE ( 'NONE', ( #4508 ), #16886, .F. ) ;
#15710 = DIRECTION ( 'NONE',  ( 1.000000000000000000, 0.000000000000000000, 0.000000000000000000 ) ) ;
#15711 = CONICAL_SURFACE ( 'NONE', #18175, 2.055000000000000160, 0.7853981633974468357 ) ;
#15712 = DIRECTION ( 'NONE',  ( -1.000000000000000000, 0.000000000000000000, -0.000000000000000000 ) ) ;
#15713 = LINE ( 'NONE', #6945, #10875 ) ;
#15714 = VECTOR ( 'NONE', #5666, 1000.000000000000114 ) ;
#15715 = EDGE_CURVE ( 'NONE', #12855, #16968, #14718, .T. ) ;
#15716 = CARTESIAN_POINT ( 'NONE',  ( 0.000000000000000000, 0.000000000000000000, 0.000000000000000000 ) ) ;
#15717 = CARTESIAN_POINT ( 'NONE',  ( 0.3170788640506440603, 13.74111462631963576, 0.1533108587036622894 ) ) ;
#15718 = DIRECTION ( 'NONE',  ( -1.000000000000000000, 0.000000000000000000, 0.000000000000000000 ) ) ;
#15719 = CARTESIAN_POINT ( 'NONE',  ( 2.747332970342022840, 11.45495994260734918, -11.66639548242795144 ) ) ;
#15720 = LINE ( 'NONE', #7038, #10276 ) ;
#15721 = ORIENTED_EDGE ( 'NONE', *, *, #14728, .T. ) ;
#15722 = B_SPLINE_CURVE_WITH_KNOTS ( 'NONE', 3,
 ( #22, #5841, #17511, #2967, #8816, #1553 ),
 .UNSPECIFIED., .F., .F.,
 ( 4, 2, 4 ),
 ( 3.903127820947815962E-18, 0.0002017457492448081235, 0.0004034914984896123438 ),
 .UNSPECIFIED. ) ;
#15723 = ORIENTED_EDGE ( 'NONE', *, *, #3300, .F. ) ;
#15724 = ORIENTED_EDGE ( 'NONE', *, *, #11066, .T. ) ;
#15725 = CONICAL_SURFACE ( 'NONE', #2311, 14.54644660717763927, 0.8559913436420816257 ) ;
#15726 = VERTEX_POINT ( 'NONE', #11669 ) ;
#15727 = AXIS2_PLACEMENT_3D ( 'NONE', #15200, #6412, #10805 ) ;
#15728 = CARTESIAN_POINT ( 'NONE',  ( -110.4113270445337918, -81.60345299795268659, -91.28051051278382033 ) ) ;
#15729 = CARTESIAN_POINT ( 'NONE',  ( 0.3095370825347234511, -13.20347358821917183, 3.806662003783360504 ) ) ;
#15730 = CARTESIAN_POINT ( 'NONE',  ( 0.3137051932979775248, -0.4596302728638797519, -13.73004976592202553 ) ) ;
#15731 = CARTESIAN_POINT ( 'NONE',  ( 0.3148213771069372502, 8.260246460850879657, -10.97836617636215628 ) ) ;
#15732 = CARTESIAN_POINT ( 'NONE',  ( 16.56872352241294521, 0.009382111268607367521, 0.004564908236399998868 ) ) ;
#15733 = ORIENTED_EDGE ( 'NONE', *, *, #11083, .F. ) ;
#15734 = CYLINDRICAL_SURFACE ( 'NONE', #13878, 5.000000000000004441 ) ;
#15735 = EDGE_CURVE ( 'NONE', #5916, #7722, #4313, .T. ) ;
#15736 = LINE ( 'NONE', #14219, #9277 ) ;
#15737 = CARTESIAN_POINT ( 'NONE',  ( 2.067729357296171688, 7.499999999999999112, -15.30380495029818988 ) ) ;
#15738 = CARTESIAN_POINT ( 'NONE',  ( 1.959212340397943786, -10.53510106265286517, 6.829000156128149257 ) ) ;
#15739 = B_SPLINE_CURVE_WITH_KNOTS ( 'NONE', 3,
 ( #9275, #15107, #3818, #771 ),
 .UNSPECIFIED., .F., .F.,
 ( 4, 4 ),
 ( 2.168404344971008868E-17, 0.003005512676784848763 ),
 .UNSPECIFIED. ) ;
#15740 = DIRECTION ( 'NONE',  ( 0.000000000000000000, 0.000000000000000000, 1.000000000000000000 ) ) ;
#15741 = EDGE_CURVE ( 'NONE', #15676, #14151, #3586, .T. ) ;
#15742 = CARTESIAN_POINT ( 'NONE',  ( 0.4862570985993235340, 13.44146924561385958, -3.580942890621532371 ) ) ;
#15743 = CARTESIAN_POINT ( 'NONE',  ( 0.4862570985993235340, 5.003653737315670647, -12.97920246947874112 ) ) ;
#15744 = AXIS2_PLACEMENT_3D ( 'NONE', #17657, #4561, #12113 ) ;
#15745 = CARTESIAN_POINT ( 'NONE',  ( 3.950837973638677170, 6.316429227969654114, -13.10350451991833687 ) ) ;
#15746 = ORIENTED_EDGE ( 'NONE', *, *, #6920, .T. ) ;
#15748 = ORIENTED_EDGE ( 'NONE', *, *, #14468, .T. ) ;
#15747 = DIRECTION ( 'NONE',  ( 1.000000000000000000, 0.000000000000000000, 0.000000000000000000 ) ) ;
#15749 = CARTESIAN_POINT ( 'NONE',  ( 16.57210152137263393, -0.01136813053532068768, -0.009075239946108325934 ) ) ;
#15750 = ORIENTED_EDGE ( 'NONE', *, *, #1186, .F. ) ;
#15751 = CARTESIAN_POINT ( 'NONE',  ( 1.847426409206446518, -0.01438352405999345808, 12.44303504652078018 ) ) ;
#15752 = ORIENTED_EDGE ( 'NONE', *, *, #6251, .F. ) ;
#15753 = CARTESIAN_POINT ( 'NONE',  ( 0.3132642857406499615, -3.740125687984641178, -13.21852905223342667 ) ) ;
#15754 = CARTESIAN_POINT ( 'NONE',  ( 0.000000000000000000, -0.8660254037844384856, -1.500000000000000000 ) ) ;
#15755 = CARTESIAN_POINT ( 'NONE',  ( 3.512766787570702487, -10.87507422923887113, -10.40533104696150701 ) ) ;
#15756 =( GEOMETRIC_REPRESENTATION_CONTEXT ( 3 ) GLOBAL_UNCERTAINTY_ASSIGNED_CONTEXT ( ( #5962 ) ) GLOBAL_UNIT_ASSIGNED_CONTEXT ( ( #7202, #5740, #7393 ) ) REPRESENTATION_CONTEXT ( 'NONE', 'WORKASPACE' ) );
#15757 = CARTESIAN_POINT ( 'NONE',  ( 1.847340342630335641, -0.1245571717074845930, -12.44248139376885831 ) ) ;
#15758 = EDGE_LOOP ( 'NONE', ( #17799, #7336, #14280, #7740 ) ) ;
#15759 = CARTESIAN_POINT ( 'NONE',  ( 1.846955891736115962, -3.593597880662430910, 11.91257079808167596 ) ) ;
#15760 = CARTESIAN_POINT ( 'NONE',  ( 1.959212340397945562, 3.239239832449027467, 12.12975361829676579 ) ) ;
#15761 = CARTESIAN_POINT ( 'NONE',  ( 1.560000000000000053, -0.8660254037844384856, 1.500000000000000000 ) ) ;
#15762 = CARTESIAN_POINT ( 'NONE',  ( 16.57778382496167424, 0.006312874906843677844, -0.01354073047775769707 ) ) ;
#15763 =( BOUNDED_SURFACE ( )  B_SPLINE_SURFACE ( 3, 1, ( 
 ( #12498, #933 ),
 ( #9538, #6774 ),
 ( #18508, #15547 ),
 ( #8122, #5417 ) ),
 .UNSPECIFIED., .F., .F., .T. ) 
 B_SPLINE_SURFACE_WITH_KNOTS ( ( 4, 4 ),
 ( 2, 2 ),
 ( 0.000000000000000000, 1.000000000000000000 ),
 ( 0.000000000000000000, 1.000000000000000000 ),
 .UNSPECIFIED. ) 
 GEOMETRIC_REPRESENTATION_ITEM ( )  RATIONAL_B_SPLINE_SURFACE ( (
 ( 1.000000000000000000, 1.000000000000000000),
 ( 0.9933953342250436691, 0.8357391271907733676),
 ( 0.9933953342250436691, 0.8357391271907733676),
 ( 1.000000000000000000, 1.000000000000000000) ) ) 
 REPRESENTATION_ITEM ( '' )  SURFACE ( )  );
#15764 = LINE ( 'NONE', #5448, #14794 ) ;
#15765 = EDGE_CURVE ( 'NONE', #8324, #15496, #14529, .T. ) ;
#15766 = AXIS2_PLACEMENT_3D ( 'NONE', #17180, #17009, #9735 ) ;
#15767 = VECTOR ( 'NONE', #13994, 1000.000000000000114 ) ;
#15768 = CONICAL_SURFACE ( 'NONE', #1730, 1732.050807568857181, 1.047197551196592746 ) ;
#15769 = CARTESIAN_POINT ( 'NONE',  ( 3.950837973638668288, 0.000000000000000000, 0.000000000000000000 ) ) ;
#15770 = CARTESIAN_POINT ( 'NONE',  ( 1.342453679581834924, 3.649820028552730022, 14.34050741580208133 ) ) ;
#15771 = ORIENTED_EDGE ( 'NONE', *, *, #8665, .T. ) ;
#15772 = CARTESIAN_POINT ( 'NONE',  ( 2.697797270744667131, -4.970631985779678352, 12.33058466479267778 ) ) ;
#15773 = VERTEX_POINT ( 'NONE', #17304 ) ;
#15774 = CIRCLE ( 'NONE', #9381, 5.000000000000000888 ) ;
#15775 = B_SPLINE_CURVE_WITH_KNOTS ( 'NONE', 3,
 ( #3327, #1910, #9074, #2010 ),
 .UNSPECIFIED., .F., .F.,
 ( 4, 4 ),
 ( 0.000000000000000000, 0.002004993803842881200 ),
 .UNSPECIFIED. ) ;
#15776 = CARTESIAN_POINT ( 'NONE',  ( 0.3148213771069381384, -12.99360322443199678, -4.463459503829131592 ) ) ;
#15777 = B_SPLINE_CURVE_WITH_KNOTS ( 'NONE', 3,
 ( #10255, #8628, #6054, #16180, #13022, #1647 ),
 .UNSPECIFIED., .F., .F.,
 ( 4, 2, 4 ),
 ( 4.014301552767626103E-17, 0.0002014099069817288116, 0.0004028198139634175078 ),
 .UNSPECIFIED. ) ;
#15778 = EDGE_LOOP ( 'NONE', ( #4765, #4864, #8408, #10233 ) ) ;
#15779 = CARTESIAN_POINT ( 'NONE',  ( 0.3145734862173253377, 4.535879238195112073, -12.96846406299301258 ) ) ;
#15780 = AXIS2_PLACEMENT_3D ( 'NONE', #11686, #10065, #11325 ) ;
#15781 = DIRECTION ( 'NONE',  ( 0.000000000000000000, 0.000000000000000000, 1.000000000000000000 ) ) ;
#15782 = VERTEX_POINT ( 'NONE', #10038 ) ;
#15783 = AXIS2_PLACEMENT_3D ( 'NONE', #10349, #16751, #15309 ) ;
#15784 = FACE_OUTER_BOUND ( 'NONE', #15504, .T. ) ;
#15785 = PRESENTATION_STYLE_ASSIGNMENT (( #10340 ) ) ;
#15786 = CARTESIAN_POINT ( 'NONE',  ( 0.3137051932979809665, -3.805684345189881856, 13.20008686438104739 ) ) ;
#15787 = CARTESIAN_POINT ( 'NONE',  ( 0.3142011359265295956, -0.3830873813805367734, -13.73310835363015059 ) ) ;
#15788 = CARTESIAN_POINT ( 'NONE',  ( 1.959283090834842644, 12.12982544407805108, 3.239245055717007826 ) ) ;
#15789 = EDGE_CURVE ( 'NONE', #14893, #15164, #15962, .T. ) ;
#15790 = ADVANCED_FACE ( 'NONE', ( #1540 ), #13745, .F. ) ;
#15791 = ORIENTED_EDGE ( 'NONE', *, *, #17255, .T. ) ;
#15792 = EDGE_CURVE ( 'NONE', #14483, #10527, #7581, .T. ) ;
#15793 = CIRCLE ( 'NONE', #8791, 14.54644660717763927 ) ;
#15794 = CARTESIAN_POINT ( 'NONE',  ( -66.35602477868047799, 14.99999999999997513, 3.000000000000002665 ) ) ;
#15795 = CARTESIAN_POINT ( 'NONE',  ( 0.4754618798421162973, -12.98792082933640835, -5.007009103465388300 ) ) ;
#15796 = CARTESIAN_POINT ( 'NONE',  ( 0.000000000000000000, -0.8660254037844384856, 1.500000000000000000 ) ) ;
#15797 = CARTESIAN_POINT ( 'NONE',  ( 16.56872352241294521, -0.01027347319884440620, 0.001821578298044753286 ) ) ;
#15798 = EDGE_LOOP ( 'NONE', ( #16785, #10309, #15482, #15673 ) ) ;
#15799 = CARTESIAN_POINT ( 'NONE',  ( 2.636624412714236865, 0.000000000000000000, 0.000000000000000000 ) ) ;
#15800 = CARTESIAN_POINT ( 'NONE',  ( 7.000000000000000000, 8.572527594031473190E-16, 8.000000000000000000 ) ) ;
#15801 = ORIENTED_EDGE ( 'NONE', *, *, #1479, .T. ) ;
#15802 = ORIENTED_EDGE ( 'NONE', *, *, #6620, .F. ) ;
#15803 = ORIENTED_EDGE ( 'NONE', *, *, #14821, .T. ) ;
#15804 = CARTESIAN_POINT ( 'NONE',  ( 8.522092701127531811, -0.3779863304871711183, 6.946128462138593918 ) ) ;
#15805 = ORIENTED_EDGE ( 'NONE', *, *, #17252, .T. ) ;
#15806 = AXIS2_PLACEMENT_3D ( 'NONE', #14833, #13848, #18424 ) ;
#15807 = FACE_OUTER_BOUND ( 'NONE', #5796, .T. ) ;
#15808 = CARTESIAN_POINT ( 'NONE',  ( 0.3145734862173233393, 13.15783074029284272, -3.953068532979860272 ) ) ;
#15809 = B_SPLINE_CURVE_WITH_KNOTS ( 'NONE', 3,
 ( #2832, #15854, #11652, #7265, #7361, #11373 ),
 .UNSPECIFIED., .F., .F.,
 ( 4, 2, 4 ),
 ( 3.551420023959826846E-17, 0.0001825746017570578021, 0.0003651492035140800965 ),
 .UNSPECIFIED. ) ;
#15810 = CARTESIAN_POINT ( 'NONE',  ( -30.00000000000000355, -12.50000000000000178, 0.000000000000000000 ) ) ;
#15811 = CARTESIAN_POINT ( 'NONE',  ( 3.950837973638676281, 14.31366178983253512, 2.591948120961855118 ) ) ;
#15812 = AXIS2_PLACEMENT_3D ( 'NONE', #8255, #3662, #6539 ) ;
#15813 = EDGE_CURVE ( 'NONE', #12599, #18854, #9181, .T. ) ;
#15814 = SURFACE_STYLE_USAGE ( .BOTH. , #1385 ) ;
#15815 = CARTESIAN_POINT ( 'NONE',  ( 2.705023505549862151, -4.909285963183986468, -12.36217802824811152 ) ) ;
#15816 = FACE_OUTER_BOUND ( 'NONE', #3174, .T. ) ;
#15817 = ADVANCED_FACE ( 'NONE', ( #15208 ), #15768, .F. ) ;
#15818 = B_SPLINE_CURVE_WITH_KNOTS ( 'NONE', 3,
 ( #16355, #17885, #12394, #3788, #15266, #2178 ),
 .UNSPECIFIED., .F., .F.,
 ( 4, 2, 4 ),
 ( 9.215718466126787689E-19, 0.001657017934710630505, 0.003314035869421260144 ),
 .UNSPECIFIED. ) ;
#15819 = CARTESIAN_POINT ( 'NONE',  ( 0.3137051932979809665, -13.20008686438108647, 3.805684345189735307 ) ) ;
#15820 = LINE ( 'NONE', #1292, #14249 ) ;
#15821 = ORIENTED_EDGE ( 'NONE', *, *, #11690, .F. ) ;
#15822 = B_SPLINE_CURVE_WITH_KNOTS ( 'NONE', 3,
 ( #15730, #13223, #11698, #4078, #4540, #138 ),
 .UNSPECIFIED., .F., .F.,
 ( 4, 2, 4 ),
 ( 2.185279341460844539E-18, 0.0002017457492448067953, 0.0004034914984896113680 ),
 .UNSPECIFIED. ) ;
#15823 = B_SPLINE_CURVE_WITH_KNOTS ( 'NONE', 3,
 ( #6427, #6334, #1739, #16644 ),
 .UNSPECIFIED., .F., .F.,
 ( 4, 4 ),
 ( 1.582786644015060892E-17, 0.003005512676784847896 ),
 .UNSPECIFIED. ) ;
#15824 = ORIENTED_EDGE ( 'NONE', *, *, #6731, .T. ) ;
#15825 = ORIENTED_EDGE ( 'NONE', *, *, #9482, .T. ) ;
#15826 = VERTEX_POINT ( 'NONE', #13766 ) ;
#15827 = ORIENTED_EDGE ( 'NONE', *, *, #17118, .T. ) ;
#15828 = CARTESIAN_POINT ( 'NONE',  ( 0.000000000000000000, 0.000000000000000000, 1.500000000000000000 ) ) ;
#15829 = CARTESIAN_POINT ( 'NONE',  ( 0.3170788640506441158, 8.200855617524535290, 11.02668139258444846 ) ) ;
#15830 = CARTESIAN_POINT ( 'NONE',  ( 2.636624412714292376, 11.60464335004048309, 11.10302021257707850 ) ) ;
#15831 = ORIENTED_EDGE ( 'NONE', *, *, #669, .T. ) ;
#15832 = DIRECTION ( 'NONE',  ( -0.000000000000000000, -0.000000000000000000, 1.000000000000000000 ) ) ;
#15833 = CARTESIAN_POINT ( 'NONE',  ( 16.57778382496167424, -0.01482878558584693925, 0.001819584982831843212 ) ) ;
#15834 = CARTESIAN_POINT ( 'NONE',  ( 3.606670283718163450, 7.499999999999999112, -16.27044756620607302 ) ) ;
#15835 = CARTESIAN_POINT ( 'NONE',  ( 16.56872352241294521, -0.009382111268607402216, -0.004564908236399935551 ) ) ;
#15836 = CIRCLE ( 'NONE', #13440, 2.500000000000000000 ) ;
#15837 = EDGE_CURVE ( 'NONE', #13196, #12599, #7333, .T. ) ;
#15838 = DIRECTION ( 'NONE',  ( 1.000000000000000000, -0.000000000000000000, -0.000000000000000000 ) ) ;
#15839 = DIRECTION ( 'NONE',  ( -1.000000000000000000, -0.000000000000000000, -0.000000000000000000 ) ) ;
#15840 = EDGE_CURVE ( 'NONE', #15520, #3962, #4789, .T. ) ;
#15841 = CARTESIAN_POINT ( 'NONE',  ( 0.3308579732647040639, 4.812490080619379995, -12.88563776947740358 ) ) ;
#15842 = DIRECTION ( 'NONE',  ( -1.000000000000000000, -0.000000000000000000, -0.000000000000000000 ) ) ;
#15843 = EDGE_LOOP ( 'NONE', ( #2792, #17556, #4728, #17843 ) ) ;
#15844 = VERTEX_POINT ( 'NONE', #13680 ) ;
#15845 = CARTESIAN_POINT ( 'NONE',  ( 16.56679352167444819, 0.009170718284672562878, -0.001518074900131760043 ) ) ;
#15846 = ORIENTED_EDGE ( 'NONE', *, *, #15126, .T. ) ;
#15847 = CIRCLE ( 'NONE', #18299, 2.699999999999999734 ) ;
#15848 = ORIENTED_EDGE ( 'NONE', *, *, #5486, .T. ) ;
#15849 = VECTOR ( 'NONE', #10389, 1000.000000000000000 ) ;
#15850 = CARTESIAN_POINT ( 'NONE',  ( -20.00000000000000000, -2.500000000000000444, -16.99999999999999645 ) ) ;
#15851 = VECTOR ( 'NONE', #10219, 1000.000000000000000 ) ;
#15852 = ADVANCED_FACE ( 'NONE', ( #13386 ), #6419, .T. ) ;
#15853 = ORIENTED_EDGE ( 'NONE', *, *, #7391, .F. ) ;
#15854 = CARTESIAN_POINT ( 'NONE',  ( 1.959283090834838426, 3.239245055717136168, -12.12982544407801555 ) ) ;
#15855 = DIRECTION ( 'NONE',  ( 0.000000000000000000, 0.000000000000000000, 1.000000000000000000 ) ) ;
#15856 = CARTESIAN_POINT ( 'NONE',  ( 16.57778382496167424, 0.006312874906843865194, 0.01354073047775895648 ) ) ;
#15857 = DIRECTION ( 'NONE',  ( -1.000000000000000000, 0.000000000000000000, 0.000000000000000000 ) ) ;
#15858 = VERTEX_POINT ( 'NONE', #11958 ) ;
#15859 = CARTESIAN_POINT ( 'NONE',  ( 1.846138399168762101, 0.4167076046097279440, -12.43476674860266051 ) ) ;
#15860 = CARTESIAN_POINT ( 'NONE',  ( 2.002547531651519996, -10.57595306287287329, -6.845637710436306200 ) ) ;
#15861 = B_SPLINE_CURVE_WITH_KNOTS ( 'NONE', 3,
 ( #4731, #16299, #3280, #13513, #4543, #240 ),
 .UNSPECIFIED., .F., .F.,
 ( 4, 2, 4 ),
 ( 4.240893905418535831E-17, 0.0002014099069817287303, 0.0004028198139634150141 ),
 .UNSPECIFIED. ) ;
#15862 = DIRECTION ( 'NONE',  ( -1.000000000000000000, -0.000000000000000000, -0.000000000000000000 ) ) ;
#15863 = CARTESIAN_POINT ( 'NONE',  ( 16.56872352241294521, -0.004564908236400289435, -0.009382111268606239951 ) ) ;
#15864 = CARTESIAN_POINT ( 'NONE',  ( 0.3307726912345235748, -3.680742887039399669, 13.25328329128664606 ) ) ;
#15865 = FILL_AREA_STYLE_COLOUR ( '', #16873 ) ;
#15866 = DIRECTION ( 'NONE',  ( 0.04547834190726749576, -0.9989653249324351725, 0.000000000000000000 ) ) ;
#15867 = CARTESIAN_POINT ( 'NONE',  ( 3.950837973638675393, 10.05648675950126325, 10.51028938476221342 ) ) ;
#15868 = SPHERICAL_SURFACE ( 'NONE', #17445, 5.315148208181397216 ) ;
#15870 = ORIENTED_EDGE ( 'NONE', *, *, #6398, .F. ) ;
#15869 = CARTESIAN_POINT ( 'NONE',  ( 2.002547531651519996, 6.845637710436190737, 10.57595306287294612 ) ) ;
#15871 = CARTESIAN_POINT ( 'NONE',  ( 0.3095370825347224519, 0.4597470195092092093, -13.73357284481724250 ) ) ;
#15872 = CARTESIAN_POINT ( 'NONE',  ( 0.3145734862173260038, -12.96846406299303212, -4.535879238195068552 ) ) ;
#15873 = EDGE_CURVE ( 'NONE', #17236, #5784, #1631, .T. ) ;
#15874 = VERTEX_POINT ( 'NONE', #9375 ) ;
#15875 = CARTESIAN_POINT ( 'NONE',  ( 1.977228804422746400, -6.152949558601968683, -14.12033626431101041 ) ) ;
#15876 =( BOUNDED_SURFACE ( )  B_SPLINE_SURFACE ( 3, 1, ( 
 ( #4206, #7169 ),
 ( #18814, #10317 ),
 ( #11655, #5710 ),
 ( #5808, #11561 ) ),
 .UNSPECIFIED., .F., .F., .T. ) 
 B_SPLINE_SURFACE_WITH_KNOTS ( ( 4, 4 ),
 ( 2, 2 ),
 ( 0.000000000000000000, 1.000000000000000000 ),
 ( 0.000000000000000000, 1.000000000000000000 ),
 .UNSPECIFIED. ) 
 GEOMETRIC_REPRESENTATION_ITEM ( )  RATIONAL_B_SPLINE_SURFACE ( (
 ( 1.000000000000000000, 1.000000000000000000),
 ( 0.9593108457356467333, 0.9995965569486454649),
 ( 0.9593108457356467333, 0.9995965569486454649),
 ( 1.000000000000000000, 1.000000000000000000) ) ) 
 REPRESENTATION_ITEM ( '' )  SURFACE ( )  );
#15877 = ORIENTED_EDGE ( 'NONE', *, *, #1998, .T. ) ;
#15878 = VECTOR ( 'NONE', #4301, 1000.000000000000000 ) ;
#15879 = CARTESIAN_POINT ( 'NONE',  ( 16.56782317627811096, -0.009228812961909619098, -0.003357783021327203059 ) ) ;
#15880 = CARTESIAN_POINT ( 'NONE',  ( 0.4862570985993252548, -3.580942890621766406, 13.44146924561379741 ) ) ;
#15881 = CARTESIAN_POINT ( 'NONE',  ( 0.3151928476913565258, -0.0002082997482820912163, -13.73922860838471927 ) ) ;
#15882 = DIRECTION ( 'NONE',  ( -1.000000000000000000, -0.000000000000000000, -0.000000000000000000 ) ) ;
#15883 = VERTEX_POINT ( 'NONE', #7579 ) ;
#15884 = CONTEXT_DEPENDENT_SHAPE_REPRESENTATION ( #16956, #9218 ) ;
#15885 =( LENGTH_UNIT ( ) NAMED_UNIT ( * ) SI_UNIT ( .MILLI., .METRE. ) );
#15886 = CARTESIAN_POINT ( 'NONE',  ( 3.074695600507268978, -2.772091048739378394, 15.30693405987788935 ) ) ;
#15888 = ORIENTED_EDGE ( 'NONE', *, *, #13925, .F. ) ;
#15887 = CARTESIAN_POINT ( 'NONE',  ( 1.342453679581834924, 9.456403821038962931, -11.38190519890843255 ) ) ;
#15889 = CARTESIAN_POINT ( 'NONE',  ( 20.00000000000000000, 2.499999999999998668, -22.00000000000000000 ) ) ;
#15890 = FACE_OUTER_BOUND ( 'NONE', #5516, .T. ) ;
#15891 = CARTESIAN_POINT ( 'NONE',  ( 3.664313757352976264, -7.012524439851403280, -12.42002390572634418 ) ) ;
#15892 = VERTEX_POINT ( 'NONE', #16552 ) ;
#15893 = CARTESIAN_POINT ( 'NONE',  ( 0.3058872367615230181, -3.664492643742856881, 13.24582953854924128 ) ) ;
#15894 = CARTESIAN_POINT ( 'NONE',  ( 1.959283090834841090, 6.829027319138399221, -10.53516775895152691 ) ) ;
#15895 = EDGE_LOOP ( 'NONE', ( #16967, #4767, #15435, #5413 ) ) ;
#15896 = EDGE_CURVE ( 'NONE', #18879, #5818, #14851, .T. ) ;
#15897 = EDGE_CURVE ( 'NONE', #17303, #9110, #6660, .T. ) ;
#15898 = EDGE_CURVE ( 'NONE', #11694, #8226, #11812, .T. ) ;
#15899 = ORIENTED_EDGE ( 'NONE', *, *, #3443, .F. ) ;
#15901 = CARTESIAN_POINT ( 'NONE',  ( 1.847421816787902404, -0.02876707915213067360, 12.44300551404155541 ) ) ;
#15900 = CIRCLE ( 'NONE', #1562, 8.767949192431123251 ) ;
#15902 = ORIENTED_EDGE ( 'NONE', *, *, #849, .F. ) ;
#15903 = CARTESIAN_POINT ( 'NONE',  ( 2.636624412714236865, 0.000000000000000000, 0.000000000000000000 ) ) ;
#15904 = EDGE_LOOP ( 'NONE', ( #9331, #12380, #4229, #16416 ) ) ;
#15905 = CARTESIAN_POINT ( 'NONE',  ( 0.3137051932979792457, 13.20008686438105983, 3.805684345189833451 ) ) ;
#15906 = CARTESIAN_POINT ( 'NONE',  ( 0.4862570985993235340, 5.003653737315670647, -12.97920246947874112 ) ) ;
#15907 = CARTESIAN_POINT ( 'NONE',  ( 1.861706995891669880, 9.751699138048550708, -7.751853334747211832 ) ) ;
#15908 = DIRECTION ( 'NONE',  ( -0.000000000000000000, 1.000000000000000000, -0.000000000000000000 ) ) ;
#15909 = EDGE_CURVE ( 'NONE', #3148, #6435, #6132, .T. ) ;
#15910 = DIRECTION ( 'NONE',  ( -1.000000000000000000, 0.000000000000000000, 0.000000000000000000 ) ) ;
#15911 = AXIS2_PLACEMENT_3D ( 'NONE', #4119, #6803, #4021 ) ;
#15912 = CARTESIAN_POINT ( 'NONE',  ( 1.918918678667043354, 10.48466773720562273, 6.832809802519053122 ) ) ;
#15913 = CARTESIAN_POINT ( 'NONE',  ( 2.123976203522053741, -10.37815841598482969, -11.67822624909937090 ) ) ;
#15914 = DIRECTION ( 'NONE',  ( -1.000000000000000000, -0.000000000000000000, -0.000000000000000000 ) ) ;
#15915 = ORIENTED_EDGE ( 'NONE', *, *, #2524, .F. ) ;
#15916 = ORIENTED_EDGE ( 'NONE', *, *, #3677, .F. ) ;
#15917 = VERTEX_POINT ( 'NONE', #10913 ) ;
#15918 = ORIENTED_EDGE ( 'NONE', *, *, #3865, .F. ) ;
#15919 = ORIENTED_EDGE ( 'NONE', *, *, #8416, .T. ) ;
#15920 = CARTESIAN_POINT ( 'NONE',  ( 1.847247051441591070, 4.004229874809190903, -11.78111530882019053 ) ) ;
#15921 = EDGE_CURVE ( 'NONE', #13362, #10401, #15976, .T. ) ;
#15922 = DIRECTION ( 'NONE',  ( -1.000000000000000000, 6.938893903907228378E-16, 0.000000000000000000 ) ) ;
#15923 = CARTESIAN_POINT ( 'NONE',  ( -32.49999999999999289, -12.50000000000000178, 3.000000000000000000 ) ) ;
#15924 = ORIENTED_EDGE ( 'NONE', *, *, #17742, .T. ) ;
#15925 = CARTESIAN_POINT ( 'NONE',  ( 0.000000000000000000, 0.000000000000000000, 8.000000000000000000 ) ) ;
#15926 = CARTESIAN_POINT ( 'NONE',  ( 8.522092701127531811, 5.841710761610186431, -3.777034505568459100 ) ) ;
#15927 = CARTESIAN_POINT ( 'NONE',  ( 5.856338620593967370, 7.500000000000129674, -12.72522090842645426 ) ) ;
#15928 = CARTESIAN_POINT ( 'NONE',  ( 16.56782317627811096, -0.006045301465876417625, 0.007739510688079494216 ) ) ;
#15929 = CARTESIAN_POINT ( 'NONE',  ( 16.56782317627811096, -0.007739510688079557534, -0.006045301465876337828 ) ) ;
#15930 = AXIS2_PLACEMENT_3D ( 'NONE', #11768, #6225, #4509 ) ;
#15931 = EDGE_CURVE ( 'NONE', #4766, #322, #4891, .T. ) ;
#15932 = CARTESIAN_POINT ( 'NONE',  ( 0.4862570985993235340, -8.769551628660655851, -10.79774104611382946 ) ) ;
#15933 = CARTESIAN_POINT ( 'NONE',  ( 1.846822687350020198, 3.566003975885688515, 11.92063725419900777 ) ) ;
#15934 = CARTESIAN_POINT ( 'NONE',  ( 0.4385251269669978580, 4.978066129061869738, -12.93791070501029239 ) ) ;
#15935 = DIRECTION ( 'NONE',  ( 0.7561779333270775005, -0.1688126975276555974, -0.6322161072786950387 ) ) ;
#15936 = ORIENTED_EDGE ( 'NONE', *, *, #10399, .F. ) ;
#15937 = VERTEX_POINT ( 'NONE', #6221 ) ;
#15938 = ORIENTED_EDGE ( 'NONE', *, *, #17349, .T. ) ;
#15939 = VERTEX_POINT ( 'NONE', #12055 ) ;
#15940 = CARTESIAN_POINT ( 'NONE',  ( 0.3058872367615226295, 13.72992299905060065, 0.6080468242581433813 ) ) ;
#15941 = ORIENTED_EDGE ( 'NONE', *, *, #3454, .F. ) ;
#15942 = CARTESIAN_POINT ( 'NONE',  ( 0.4862570985993235340, -13.44146924561378498, -3.580942890621813923 ) ) ;
#15943 = EDGE_CURVE ( 'NONE', #2897, #7741, #15739, .T. ) ;
#15944 = CARTESIAN_POINT ( 'NONE',  ( -66.35602477868047799, -10.00000000000000888, 5.999999999999999112 ) ) ;
#15945 = CARTESIAN_POINT ( 'NONE',  ( 2.636624412715138366, -11.10302021257964888, 11.60464335004044223 ) ) ;
#15946 = CARTESIAN_POINT ( 'NONE',  ( 8.438534575730034959, -2.341351102130323714, 6.454982381540280478 ) ) ;
#15947 = ORIENTED_EDGE ( 'NONE', *, *, #18806, .F. ) ;
#15948 = CYLINDRICAL_SURFACE ( 'NONE', #4408, 5.000000000000000000 ) ;
#15949 = VECTOR ( 'NONE', #120, 1000.000000000000000 ) ;
#15950 = CARTESIAN_POINT ( 'NONE',  ( 0.3137051932979792457, 13.73004976592202198, 0.4596302728640249136 ) ) ;
#15951 = CARTESIAN_POINT ( 'NONE',  ( 0.3151928476913592458, -13.73922860838471749, 0.0002082997483299325046 ) ) ;
#15952 = CARTESIAN_POINT ( 'NONE',  ( 16.56679352167444819, -0.004162264567719712108, -0.008311568981097318051 ) ) ;
#15953 = ADVANCED_FACE ( 'NONE', ( #17890 ), #18837, .F. ) ;
#15954 = CARTESIAN_POINT ( 'NONE',  ( 0.000000000000000000, 0.000000000000000000, 0.000000000000000000 ) ) ;
#15955 = CARTESIAN_POINT ( 'NONE',  ( 3.664313757352976264, 1.627055439596472475, -14.16986885736090329 ) ) ;
#15956 = EDGE_CURVE ( 'NONE', #14563, #11376, #2306, .T. ) ;
#15957 = CARTESIAN_POINT ( 'NONE',  ( 16.56753206892534891, 0.001549402974394159613, 0.009369540855502535986 ) ) ;
#15958 = VERTEX_POINT ( 'NONE', #9816 ) ;
#15959 = DIRECTION ( 'NONE',  ( 1.000000000000000000, 0.000000000000000000, 0.000000000000000000 ) ) ;
#15961 = VERTEX_POINT ( 'NONE', #9644 ) ;
#15960 = CARTESIAN_POINT ( 'NONE',  ( 1.846524061778019199, 0.3544704288994222074, -12.43723828841088164 ) ) ;
#15962 = LINE ( 'NONE', #9, #17923 ) ;
#15963 = CIRCLE ( 'NONE', #18108, 2.600000000000092015 ) ;
#15964 = DIRECTION ( 'NONE',  ( 0.000000000000000000, -0.5000000000000003331, -0.8660254037844383745 ) ) ;
#15965 = ORIENTED_EDGE ( 'NONE', *, *, #10810, .F. ) ;
#15966 = CARTESIAN_POINT ( 'NONE',  ( 0.3151926232592475174, 4.172630140040981317, -13.09050869763088443 ) ) ;
#15967 = CARTESIAN_POINT ( 'NONE',  ( 6.538348415311014072, -7.500000000000000888, -17.00000000000000000 ) ) ;
#15968 = ORIENTED_EDGE ( 'NONE', *, *, #1748, .F. ) ;
#15969 = CARTESIAN_POINT ( 'NONE',  ( 0.3170788640506440603, 13.02120094575828269, 4.392045232375855868 ) ) ;
#15970 = CYLINDRICAL_SURFACE ( 'NONE', #15251, 5.000000000000000888 ) ;
#15971 = CARTESIAN_POINT ( 'NONE',  ( 1.846138399168762101, -9.815003036200353748, -7.646096044340000120 ) ) ;
#15972 = DIRECTION ( 'NONE',  ( -1.000000000000000000, 0.000000000000000000, -0.000000000000000000 ) ) ;
#15973 = VECTOR ( 'NONE', #4118, 1000.000000000000000 ) ;
#15974 = ORIENTED_EDGE ( 'NONE', *, *, #13893, .F. ) ;
#15975 = ADVANCED_FACE ( 'NONE', ( #15648 ), #4437, .F. ) ;
#15976 = B_SPLINE_CURVE_WITH_KNOTS ( 'NONE', 3,
 ( #13479, #304, #17984, #10525, #16360, #3239 ),
 .UNSPECIFIED., .F., .F.,
 ( 4, 2, 4 ),
 ( 2.474737474518078493E-18, 0.0002017457492448081235, 0.0004034914984896138075 ),
 .UNSPECIFIED. ) ;
#15977 = DIRECTION ( 'NONE',  ( 0.000000000000000000, 0.000000000000000000, 1.000000000000000000 ) ) ;
#15978 = ADVANCED_FACE ( 'NONE', ( #18529 ), #3571, .T. ) ;
#15979 = FACE_BOUND ( 'NONE', #3900, .T. ) ;
#15980 = CARTESIAN_POINT ( 'NONE',  ( 16.58200780006414732, -0.0006320991582348829945, 0.01115192838421569070 ) ) ;
#15981 = CARTESIAN_POINT ( 'NONE',  ( 16.57778382496167424, 0.006312874906843865194, 0.01354073047775895648 ) ) ;
#15982 = ORIENTED_EDGE ( 'NONE', *, *, #10849, .T. ) ;
#15983 = CARTESIAN_POINT ( 'NONE',  ( 2.353870697619110608, -10.00946331859657334, -8.216087327473042379 ) ) ;
#15984 = CARTESIAN_POINT ( 'NONE',  ( 0.4862570985993235340, -13.89016912371018186, 0.7479633556561964269 ) ) ;
#15985 = EDGE_LOOP ( 'NONE', ( #5343, #5930, #9271, #18245 ) ) ;
#15986 = ORIENTED_EDGE ( 'NONE', *, *, #17591, .F. ) ;
#15987 = CARTESIAN_POINT ( 'NONE',  ( 2.747332970342022840, -11.66639548242815572, 11.45495994260713957 ) ) ;
#15988 = VECTOR ( 'NONE', #6118, 1000.000000000000114 ) ;
#15989 = CIRCLE ( 'NONE', #10505, 5.000000000000000888 ) ;
#15990 = ORIENTED_EDGE ( 'NONE', *, *, #71, .F. ) ;
#15991 = CARTESIAN_POINT ( 'NONE',  ( 0.3137051932979792457, -0.4596302728640728752, 13.73004976592201842 ) ) ;
#15992 = ORIENTED_EDGE ( 'NONE', *, *, #1098, .T. ) ;
#15993 = DIRECTION ( 'NONE',  ( -1.000000000000000000, -0.000000000000000000, -0.000000000000000000 ) ) ;
#15994 = CARTESIAN_POINT ( 'NONE',  ( 1.847412631396500249, -10.04119192206681177, -7.348689888531952263 ) ) ;
#15995 = CYLINDRICAL_SURFACE ( 'NONE', #14193, 5.000000000000000000 ) ;
#15996 = CARTESIAN_POINT ( 'NONE',  ( 1.500000000000000000, 2.869946927167511679E-16, 5.000000000000000000 ) ) ;
#15997 = EDGE_CURVE ( 'NONE', #17750, #12252, #862, .T. ) ;
#15998 = EDGE_CURVE ( 'NONE', #5926, #18142, #12798, .T. ) ;
#15999 = CARTESIAN_POINT ( 'NONE',  ( 0.4754618798421171855, -13.89949764182683190, 0.7484603771383911974 ) ) ;
#16000 = ADVANCED_FACE ( 'NONE', ( #8135 ), #8450, .T. ) ;
#16001 = CARTESIAN_POINT ( 'NONE',  ( 0.4862570985993235340, -10.79774104611366781, -8.769551628660854803 ) ) ;
#16002 = CARTESIAN_POINT ( 'NONE',  ( 0.4385251269669942498, 7.540955776459739468, 11.63205320541525900 ) ) ;
#16003 = AXIS2_PLACEMENT_3D ( 'NONE', #1139, #18350, #2385 ) ;
#16004 = DIRECTION ( 'NONE',  ( -0.000000000000000000, -0.5000000000000003331, -0.8660254037844384856 ) ) ;
#16005 = EDGE_LOOP ( 'NONE', ( #325, #16520, #7604, #11162 ) ) ;
#16006 = CIRCLE ( 'NONE', #466, 2.600000000000092015 ) ;
#16007 = ORIENTED_EDGE ( 'NONE', *, *, #7216, .T. ) ;
#16008 = ORIENTED_EDGE ( 'NONE', *, *, #4025, .T. ) ;
#16009 = VERTEX_POINT ( 'NONE', #15563 ) ;
#16010 = ORIENTED_EDGE ( 'NONE', *, *, #404, .F. ) ;
#16011 = B_SPLINE_CURVE_WITH_KNOTS ( 'NONE', 3,
 ( #124, #6150, #3063, #17422 ),
 .UNSPECIFIED., .F., .F.,
 ( 4, 4 ),
 ( 0.000000000000000000, 0.002004993803842607548 ),
 .UNSPECIFIED. ) ;
#16012 = CARTESIAN_POINT ( 'NONE',  ( 0.3151930723728413319, -8.013866567350813597, -11.16020735774775829 ) ) ;
#16013 = AXIS2_PLACEMENT_3D ( 'NONE', #1355, #7198, #15972 ) ;
#16014 = CARTESIAN_POINT ( 'NONE',  ( 0.3170788640506440603, 7.952793437297573931, 11.20690911610906326 ) ) ;
#16015 = AXIS2_PLACEMENT_3D ( 'NONE', #12989, #13470, #14906 ) ;
#16016 = CARTESIAN_POINT ( 'NONE',  ( 3.512766787570810401, -2.025881399556277440, -14.91422000116817159 ) ) ;
#16017 = EDGE_LOOP ( 'NONE', ( #12312, #4673, #13146, #10113 ) ) ;
#16018 = PLANE ( 'NONE',  #2283 ) ;
#16019 = AXIS2_PLACEMENT_3D ( 'NONE', #14992, #380, #13752 ) ;
#16020 = CARTESIAN_POINT ( 'NONE',  ( 0.4754618798421167414, -0.7484603771385368587, 13.89949764182682301 ) ) ;
#16021 = LINE ( 'NONE', #4565, #1197 ) ;
#16022 = DIRECTION ( 'NONE',  ( -1.000000000000000000, -0.000000000000000000, -0.000000000000000000 ) ) ;
#16023 = CARTESIAN_POINT ( 'NONE',  ( 3.950837973638668288, 0.000000000000000000, 0.000000000000000000 ) ) ;
#16024 = EDGE_CURVE ( 'NONE', #10648, #18779, #6979, .T. ) ;
#16025 = EDGE_CURVE ( 'NONE', #14890, #10313, #9663, .T. ) ;
#16026 = FACE_OUTER_BOUND ( 'NONE', #604, .T. ) ;
#16027 = CARTESIAN_POINT ( 'NONE',  ( 1.977436885026095270, -6.153171729168663617, 14.12046670317548980 ) ) ;
#16028 = ADVANCED_FACE ( 'NONE', ( #14128 ), #6410, .F. ) ;
#16029 = LINE ( 'NONE', #4374, #4612 ) ;
#16030 = ADVANCED_FACE ( 'NONE', ( #18613 ), #8352, .F. ) ;
#16031 = SPHERICAL_SURFACE ( 'NONE', #528, 5.000000000000000000 ) ;
#16032 = ORIENTED_EDGE ( 'NONE', *, *, #5861, .F. ) ;
#16033 = VECTOR ( 'NONE', #12550, 1000.000000000000000 ) ;
#16034 = CIRCLE ( 'NONE', #7823, 5.000000000000000000 ) ;
#16035 = ORIENTED_EDGE ( 'NONE', *, *, #11357, .T. ) ;
#16036 = VERTEX_POINT ( 'NONE', #9919 ) ;
#16037 = ORIENTED_EDGE ( 'NONE', *, *, #9265, .F. ) ;
#16038 = CARTESIAN_POINT ( 'NONE',  ( 16.56872352241294521, 0.004907101719995680782, 0.009207754980064214098 ) ) ;
#16039 = ORIENTED_EDGE ( 'NONE', *, *, #8884, .T. ) ;
#16040 = CARTESIAN_POINT ( 'NONE',  ( 0.4862570985993235340, -3.580942890621579444, -13.44146924561384537 ) ) ;
#16041 = CARTESIAN_POINT ( 'NONE',  ( 1.847034903785822246, 11.76058231742745797, 4.063013886994747637 ) ) ;
#16042 = CARTESIAN_POINT ( 'NONE',  ( 2.123976203522053297, 15.26039569100264082, -3.347755036805743600 ) ) ;
#16043 = CARTESIAN_POINT ( 'NONE',  ( 2.002547531651519996, -12.17374746633575988, -3.242439124566779185 ) ) ;
#16044 = VERTEX_POINT ( 'NONE', #9040 ) ;
#16045 = CARTESIAN_POINT ( 'NONE',  ( 16.57210152137263393, -0.009075239946109120437, -0.01136813053532156892 ) ) ;
#16046 = DIRECTION ( 'NONE',  ( 0.7561779333270775005, 0.3559159372837274460, 0.5491072561318377510 ) ) ;
#16047 = VECTOR ( 'NONE', #18149, 1000.000000000000000 ) ;
#16048 = CARTESIAN_POINT ( 'NONE',  ( 16.56872352241294521, 0.007512283835804314455, -0.007240717549633915451 ) ) ;
#16049 =( GEOMETRIC_REPRESENTATION_CONTEXT ( 3 ) GLOBAL_UNCERTAINTY_ASSIGNED_CONTEXT ( ( #16266 ) ) GLOBAL_UNIT_ASSIGNED_CONTEXT ( ( #6264, #2155, #540 ) ) REPRESENTATION_CONTEXT ( 'NONE', 'WORKASPACE' ) );
#16050 = CIRCLE ( 'NONE', #2863, 14.54644660717763927 ) ;
#16051 = DIRECTION ( 'NONE',  ( 0.000000000000000000, 0.5150380749100523792, 0.8571673007021134438 ) ) ;
#16052 = CARTESIAN_POINT ( 'NONE',  ( 3.353306896162453921, -13.88482890973695660, -1.348936822032970495 ) ) ;
#16053 = B_SPLINE_CURVE_WITH_KNOTS ( 'NONE', 3,
 ( #3910, #11364, #7255, #9812 ),
 .UNSPECIFIED., .F., .F.,
 ( 4, 4 ),
 ( 2.298835888684693015E-16, 0.002004993803842571552 ),
 .UNSPECIFIED. ) ;
#16054 = FACE_OUTER_BOUND ( 'NONE', #15626, .T. ) ;
#16055 = VERTEX_POINT ( 'NONE', #1781 ) ;
#16056 = EDGE_CURVE ( 'NONE', #9114, #7547, #15459, .T. ) ;
#16057 = CARTESIAN_POINT ( 'NONE',  ( 2.002547531651519996, -9.778737580845755062, 7.942910686618138705 ) ) ;
#16059 = VERTEX_POINT ( 'NONE', #2735 ) ;
#16058 = CARTESIAN_POINT ( 'NONE',  ( 2.705023505549863039, 10.24007717649592841, -8.489131503859667305 ) ) ;
#16060 = CARTESIAN_POINT ( 'NONE',  ( 0.3095370825347233956, 3.806662003783596759, -13.20347358821910433 ) ) ;
#16061 = AXIS2_PLACEMENT_3D ( 'NONE', #17528, #4436, #4060 ) ;
#16062 = CARTESIAN_POINT ( 'NONE',  ( 2.636624412714236865, 0.000000000000000000, 0.000000000000000000 ) ) ;
#16063 = VERTEX_POINT ( 'NONE', #11814 ) ;
#16064 = CARTESIAN_POINT ( 'NONE',  ( 3.950837973638676281, -12.81214529934979929, 6.888253895133251703 ) ) ;
#16065 = PRODUCT_DEFINITION_SHAPE ( 'NONE', 'NONE',  #11634 ) ;
#16066 = CARTESIAN_POINT ( 'NONE',  ( 2.117882332754172037, -7.500000000000000888, -15.34025089741903081 ) ) ;
#16067 = EDGE_LOOP ( 'NONE', ( #16010, #15802, #2741, #2775 ) ) ;
#16068 = CARTESIAN_POINT ( 'NONE',  ( 0.3720661004400037664, 7.524064345033464107, 11.58636699658217672 ) ) ;
#16069 = SURFACE_STYLE_FILL_AREA ( #8526 ) ;
#16070 = EDGE_CURVE ( 'NONE', #620, #18610, #18065, .T. ) ;
#16071 = VECTOR ( 'NONE', #12328, 1000.000000000000000 ) ;
#16072 = DIRECTION ( 'NONE',  ( 0.7561779333270775005, -0.1688126975276555974, -0.6322161072786950387 ) ) ;
#16073 = FACE_OUTER_BOUND ( 'NONE', #7262, .T. ) ;
#16074 = VECTOR ( 'NONE', #13720, 1000.000000000000227 ) ;
#16075 = MECHANICAL_DESIGN_GEOMETRIC_PRESENTATION_REPRESENTATION (  '', ( #9957 ), #14544 ) ;
#16076 = PRODUCT_DEFINITION ( 'UNKNOWN', '', #10827, #4852 ) ;
#16077 = ITEM_DEFINED_TRANSFORMATION ( 'NONE', 'NONE', #13652,  #2030 ) ;
#16078 = ADVANCED_FACE ( 'NONE', ( #10377 ), #817, .T. ) ;
#16079 = ADVANCED_FACE ( 'NONE', ( #8582 ), #15680, .F. ) ;
#16080 = VECTOR ( 'NONE', #10996, 1000.000000000000000 ) ;
#16081 = SURFACE_STYLE_USAGE ( .BOTH. , #1551 ) ;
#16083 = AXIS2_PLACEMENT_3D ( 'NONE', #1636, #10244, #5832 ) ;
#16082 = CARTESIAN_POINT ( 'NONE',  ( 3.074695600507159732, -15.30693405987801370, -2.772091048739451669 ) ) ;
#16084 = DIRECTION ( 'NONE',  ( 1.000000000000000000, 0.000000000000000000, -0.000000000000000000 ) ) ;
#16085 = DIRECTION ( 'NONE',  ( 1.000000000000000000, 0.000000000000000000, 0.000000000000000000 ) ) ;
#16086 = DIRECTION ( 'NONE',  ( -1.000000000000000000, 1.040834085586084059E-15, 0.000000000000000000 ) ) ;
#16087 = CARTESIAN_POINT ( 'NONE',  ( 1.845755665166723736, -12.43231320373360482, -0.4784952423729852966 ) ) ;
#16088 = AXIS2_PLACEMENT_3D ( 'NONE', #8271, #14087, #2241 ) ;
#16089 = ORIENTED_EDGE ( 'NONE', *, *, #17354, .F. ) ;
#16090 = CARTESIAN_POINT ( 'NONE',  ( 1.918918678667047129, 4.466049546133911363, 11.69059232068580556 ) ) ;
#16091 = CARTESIAN_POINT ( 'NONE',  ( 1.562796894703937678, 4.769696007084728073, 1.500000000000000000 ) ) ;
#16092 = ORIENTED_EDGE ( 'NONE', *, *, #9862, .F. ) ;
#16093 = AXIS2_PLACEMENT_3D ( 'NONE', #9012, #4421, #10445 ) ;
#16094 = MECHANICAL_DESIGN_GEOMETRIC_PRESENTATION_REPRESENTATION (  '', ( #10609 ), #14867 ) ;
#16095 = ORIENTED_EDGE ( 'NONE', *, *, #15403, .F. ) ;
#16096 = CARTESIAN_POINT ( 'NONE',  ( 16.58200780006414732, 0.0006320991582340733123, 0.01115192838421469670 ) ) ;
#16097 = EDGE_LOOP ( 'NONE', ( #3998, #3118, #13530, #14636 ) ) ;
#16098 = DIRECTION ( 'NONE',  ( -0.000000000000000000, 1.000000000000000000, -0.000000000000000000 ) ) ;
#16099 = ORIENTED_EDGE ( 'NONE', *, *, #6353, .T. ) ;
#16100 = ADVANCED_FACE ( 'NONE', ( #444 ), #10304, .F. ) ;
#16101 = CARTESIAN_POINT ( 'NONE',  ( 0.4754618798421162973, 5.007009103465249744, 12.98792082933646341 ) ) ;
#16102 = CARTESIAN_POINT ( 'NONE',  ( 16.57778382496167424, 0.01354073047775893567, -0.006312874906843913766 ) ) ;
#16103 = CARTESIAN_POINT ( 'NONE',  ( 0.3170788640506441158, 0.1533108587036162707, 13.74111462631963576 ) ) ;
#16104 = CARTESIAN_POINT ( 'NONE',  ( 0.000000000000000000, 0.000000000000000000, 8.000000000000000000 ) ) ;
#16105 = UNCERTAINTY_MEASURE_WITH_UNIT (LENGTH_MEASURE( 1.000000000000000082E-05 ), #3649, 'distance_accuracy_value', 'NONE');
#16106 = ADVANCED_FACE ( 'NONE', ( #11457 ), #1317, .T. ) ;
#16107 = CARTESIAN_POINT ( 'NONE',  ( 16.56872352241294521, -0.009207754980063714498, -0.004907101719994726684 ) ) ;
#16108 = FACE_OUTER_BOUND ( 'NONE', #3448, .T. ) ;
#16109 = CARTESIAN_POINT ( 'NONE',  ( 0.3132642857406499615, -3.740125687984641178, -13.21852905223342667 ) ) ;
#16110 = CARTESIAN_POINT ( 'NONE',  ( 3.377929128793395908, -3.070552481924963217, 13.64476897106782971 ) ) ;
#16111 = CARTESIAN_POINT ( 'NONE',  ( 0.3132642857406501835, 7.641821025099867271, 11.41580579227779779 ) ) ;
#16112 = CARTESIAN_POINT ( 'NONE',  ( 1.560000000000000053, -1.732050807568877859, -1.752539433813135784E-17 ) ) ;
#16113 = ORIENTED_EDGE ( 'NONE', *, *, #10782, .T. ) ;
#16114 = CARTESIAN_POINT ( 'NONE',  ( 16.56872352241294521, 0.007512283835804314455, -0.007240717549633915451 ) ) ;
#16115 = EDGE_LOOP ( 'NONE', ( #7897, #10073, #15059, #11893 ) ) ;
#16116 = VECTOR ( 'NONE', #8466, 1000.000000000000000 ) ;
#16117 = VERTEX_POINT ( 'NONE', #7160 ) ;
#16118 = ORIENTED_EDGE ( 'NONE', *, *, #1206, .F. ) ;
#16119 = VERTEX_POINT ( 'NONE', #7717 ) ;
#16120 = ADVANCED_FACE ( 'NONE', ( #13525 ), #12259, .F. ) ;
#16121 = CARTESIAN_POINT ( 'NONE',  ( 1.846138399168762101, -9.815003036200353748, -7.646096044340000120 ) ) ;
#16122 = CARTESIAN_POINT ( 'NONE',  ( 1.977228804422746400, -6.152949558601968683, -14.12033626431101041 ) ) ;
#16123 = CARTESIAN_POINT ( 'NONE',  ( 0.4862570985993252548, 10.79774104611373353, 8.769551628660776643 ) ) ;
#16124 = ORIENTED_EDGE ( 'NONE', *, *, #7829, .F. ) ;
#16125 = CARTESIAN_POINT ( 'NONE',  ( -27.50000000000000711, -12.50000000000000178, 6.000000000000000000 ) ) ;
#16126 = CARTESIAN_POINT ( 'NONE',  ( -66.35602477868047799, 9.999999999999973355, 5.999999999999999112 ) ) ;
#16127 = FACE_OUTER_BOUND ( 'NONE', #6064, .T. ) ;
#16128 = CARTESIAN_POINT ( 'NONE',  ( 3.512766787570899663, 10.87507422923878586, 10.40533104696127076 ) ) ;
#16129 = CARTESIAN_POINT ( 'NONE',  ( 3.950837973638675393, -10.05648675950118509, -10.51028938476228980 ) ) ;
#16130 = CARTESIAN_POINT ( 'NONE',  ( 3.074695600507694859, 14.01296402267844066, 6.754521329824622278 ) ) ;
#16131 = CARTESIAN_POINT ( 'NONE',  ( 1.846138399168762989, 3.446241763652997836, 11.95493567637851839 ) ) ;
#16132 = CARTESIAN_POINT ( 'NONE',  ( 0.3148208552358962020, -11.24855514421869529, -7.888357771040825028 ) ) ;
#16133 = CARTESIAN_POINT ( 'NONE',  ( 1.846524061778018977, 7.023652644192272199, 10.27028962889599484 ) ) ;
#16134 = ORIENTED_EDGE ( 'NONE', *, *, #2270, .F. ) ;
#16135 = ORIENTED_EDGE ( 'NONE', *, *, #6885, .T. ) ;
#16136 = EDGE_LOOP ( 'NONE', ( #10479, #15450, #13537, #3845 ) ) ;
#16137 = ORIENTED_EDGE ( 'NONE', *, *, #8189, .T. ) ;
#16138 = FACE_OUTER_BOUND ( 'NONE', #5299, .T. ) ;
#16139 = EDGE_CURVE ( 'NONE', #5819, #12351, #16311, .T. ) ;
#16140 = ORIENTED_EDGE ( 'NONE', *, *, #12102, .F. ) ;
#16141 = EDGE_CURVE ( 'NONE', #5568, #9336, #7815, .T. ) ;
#16142 = ADVANCED_FACE ( 'NONE', ( #13900 ), #18226, .F. ) ;
#16143 = CARTESIAN_POINT ( 'NONE',  ( 3.950837973638668288, 0.000000000000000000, 0.000000000000000000 ) ) ;
#16144 = CARTESIAN_POINT ( 'NONE',  ( 2.320520222537238553, -13.71278186123262799, 7.743191299717230969 ) ) ;
#16145 = CARTESIAN_POINT ( 'NONE',  ( 0.3058872367615230181, 4.821066432589326212, 12.87003593440630311 ) ) ;
#16146 = PLANE ( 'NONE',  #167 ) ;
#16147 = EDGE_LOOP ( 'NONE', ( #3468, #12832 ) ) ;
#16148 = CARTESIAN_POINT ( 'NONE',  ( 3.353306896162455697, 7.069984850384810393, 12.02594772223098651 ) ) ;
#16149 = CARTESIAN_POINT ( 'NONE',  ( 1.846138399168762989, 3.446241763652997836, 11.95493567637851839 ) ) ;
#16150 = CARTESIAN_POINT ( 'NONE',  ( -6.538348415311011408, 2.499999999999998224, -12.00000000000000000 ) ) ;
#16151 = CARTESIAN_POINT ( 'NONE',  ( 0.8740779401512879243, 13.31469722824398794, -5.211551231203936929 ) ) ;
#16152 = DIRECTION ( 'NONE',  ( 0.000000000000000000, 0.000000000000000000, 1.000000000000000000 ) ) ;
#16153 = ORIENTED_EDGE ( 'NONE', *, *, #10957, .T. ) ;
#16154 = MANIFOLD_SOLID_BREP ( 'M5 Clearance Hole1', #14868 ) ;
#16155 = AXIS2_PLACEMENT_3D ( 'NONE', #3203, #3307, #9052 ) ;
#16156 = CARTESIAN_POINT ( 'NONE',  ( 0.8740764193767259771, -13.31469591265765118, -5.211550415969147920 ) ) ;
#16157 = VECTOR ( 'NONE', #115, 1000.000000000000000 ) ;
#16159 = ORIENTED_EDGE ( 'NONE', *, *, #1160, .T. ) ;
#16158 = CARTESIAN_POINT ( 'NONE',  ( 0.000000000000000000, 0.000000000000000000, 3.000000000000000000 ) ) ;
#16160 = CARTESIAN_POINT ( 'NONE',  ( 1.104287921197080512E-14, -9.013167318348349610, 22.41316734529519650 ) ) ;
#16161 = CARTESIAN_POINT ( 'NONE',  ( 0.3058872367615226295, 11.46514199369368825, -7.578326039752480092 ) ) ;
#16162 =( BOUNDED_SURFACE ( )  B_SPLINE_SURFACE ( 3, 1, ( 
 ( #11544, #9053 ),
 ( #15928, #17363 ),
 ( #2817, #1595 ),
 ( #11921, #14882 ) ),
 .UNSPECIFIED., .F., .F., .T. ) 
 B_SPLINE_SURFACE_WITH_KNOTS ( ( 4, 4 ),
 ( 2, 2 ),
 ( 0.000000000000000000, 1.000000000000000000 ),
 ( 0.000000000000000000, 1.000000000000000000 ),
 .UNSPECIFIED. ) 
 GEOMETRIC_REPRESENTATION_ITEM ( )  RATIONAL_B_SPLINE_SURFACE ( (
 ( 1.000000000000000000, 1.000000000000000000),
 ( 0.9933953342250436691, 0.8357391271907733676),
 ( 0.9933953342250436691, 0.8357391271907733676),
 ( 1.000000000000000000, 1.000000000000000000) ) ) 
 REPRESENTATION_ITEM ( '' )  SURFACE ( )  );
#16163 = CIRCLE ( 'NONE', #3953, 5.000000000000004441 ) ;
#16164 = EDGE_LOOP ( 'NONE', ( #11188, #2553, #11494, #5776 ) ) ;
#16165 = DIRECTION ( 'NONE',  ( -0.000000000000000000, 0.5000000000000003331, -0.8660254037844384856 ) ) ;
#16166 = CARTESIAN_POINT ( 'NONE',  ( 5.343731732830336867, -7.500000000000000888, -16.88485148858663365 ) ) ;
#16167 = VERTEX_POINT ( 'NONE', #16866 ) ;
#16168 = CARTESIAN_POINT ( 'NONE',  ( 2.002547531651519996, 7.942910686618313676, -9.778737580845612953 ) ) ;
#16169 = PLANE ( 'NONE',  #9739 ) ;
#16170 = EDGE_CURVE ( 'NONE', #9139, #8437, #9330, .T. ) ;
#16171 = DIRECTION ( 'NONE',  ( 0.000000000000000000, 0.000000000000000000, 1.000000000000000000 ) ) ;
#16172 = CARTESIAN_POINT ( 'NONE',  ( 0.000000000000000000, 2.499999999999998668, -22.00000000000000000 ) ) ;
#16173 = ADVANCED_FACE ( 'NONE', ( #9510 ), #14204, .F. ) ;
#16174 = VERTEX_POINT ( 'NONE', #12469 ) ;
#16175 = ADVANCED_FACE ( 'NONE', ( #3591 ), #1141, .F. ) ;
#16176 = CARTESIAN_POINT ( 'NONE',  ( 0.3170788640506441158, -8.200855617524453578, -11.02668139258451063 ) ) ;
#16177 = FACE_OUTER_BOUND ( 'NONE', #7977, .T. ) ;
#16178 = CARTESIAN_POINT ( 'NONE',  ( 0.3095370825347233956, -0.4597470195089253808, -13.73357284481725316 ) ) ;
#16179 = FACE_OUTER_BOUND ( 'NONE', #10070, .T. ) ;
#16180 = CARTESIAN_POINT ( 'NONE',  ( 0.3308579732647042304, 7.595989242675130093, 11.46737410776356469 ) ) ;
#16181 = ORIENTED_EDGE ( 'NONE', *, *, #440, .F. ) ;
#16182 = CARTESIAN_POINT ( 'NONE',  ( 3.377929128793398572, 12.84367544717943410, -5.536064832134035996 ) ) ;
#16183 = DIRECTION ( 'NONE',  ( -1.000000000000000000, -0.000000000000000000, -0.000000000000000000 ) ) ;
#16184 = EDGE_LOOP ( 'NONE', ( #9950, #770, #10963 ) ) ;
#16185 = ORIENTED_EDGE ( 'NONE', *, *, #10097, .T. ) ;
#16186 = CARTESIAN_POINT ( 'NONE',  ( 0.4862570985993235340, -5.003653737315397976, -12.97920246947884770 ) ) ;
#16187 = B_SPLINE_CURVE_WITH_KNOTS ( 'NONE', 3,
 ( #4079, #14308, #16016, #3004 ),
 .UNSPECIFIED., .F., .F.,
 ( 4, 4 ),
 ( 3.750785467376078809E-16, 0.002004993803842428438 ),
 .UNSPECIFIED. ) ;
#16188 = ORIENTED_EDGE ( 'NONE', *, *, #17188, .F. ) ;
#16189 = FACE_OUTER_BOUND ( 'NONE', #12488, .T. ) ;
#16190 = EDGE_CURVE ( 'NONE', #8004, #13362, #2075, .T. ) ;
#16191 = ORIENTED_EDGE ( 'NONE', *, *, #10946, .F. ) ;
#16192 = CARTESIAN_POINT ( 'NONE',  ( 1.847168016377981115, 9.955470380986737311, -7.464000291196308368 ) ) ;
#16193 = EDGE_CURVE ( 'NONE', #2734, #2050, #6421, .T. ) ;
#16194 = EDGE_CURVE ( 'NONE', #10257, #11324, #12379, .T. ) ;
#16195 = CARTESIAN_POINT ( 'NONE',  ( 0.3095370825347233956, -13.73357284481725138, 0.4597470195089733425 ) ) ;
#16196 = DIRECTION ( 'NONE',  ( -0.000000000000000000, 0.000000000000000000, 1.000000000000000000 ) ) ;
#16197 = CARTESIAN_POINT ( 'NONE',  ( 0.4754618798421167414, -7.564402563418384240, -11.68486377711974811 ) ) ;
#16198 = CARTESIAN_POINT ( 'NONE',  ( 16.56753206892534891, -0.009369540855502119653, -0.001549402974393242162 ) ) ;
#16200 = LINE ( 'NONE', #13326, #7821 ) ;
#16199 =( BOUNDED_SURFACE ( )  B_SPLINE_SURFACE ( 3, 1, ( 
 ( #1692, #17462 ),
 ( #1794, #7636 ),
 ( #13446, #6186 ),
 ( #16222, #359 ) ),
 .UNSPECIFIED., .F., .F., .T. ) 
 B_SPLINE_SURFACE_WITH_KNOTS ( ( 4, 4 ),
 ( 2, 2 ),
 ( 0.000000000000000000, 1.000000000000000000 ),
 ( 0.000000000000000000, 1.000000000000000000 ),
 .UNSPECIFIED. ) 
 GEOMETRIC_REPRESENTATION_ITEM ( )  RATIONAL_B_SPLINE_SURFACE ( (
 ( 1.000000000000000000, 1.000000000000000000),
 ( 0.9933953342250436691, 0.8357391271907733676),
 ( 0.9933953342250436691, 0.8357391271907733676),
 ( 1.000000000000000000, 1.000000000000000000) ) ) 
 REPRESENTATION_ITEM ( '' )  SURFACE ( )  );
#16201 = CARTESIAN_POINT ( 'NONE',  ( 1.847426409206450959, -2.029922383240494730E-11, 12.44303504652081038 ) ) ;
#16202 = CARTESIAN_POINT ( 'NONE',  ( 0.3137051932979792457, 4.679953077377485116, 12.91601973349272114 ) ) ;
#16203 = DIRECTION ( 'NONE',  ( 0.000000000000000000, 0.000000000000000000, 1.000000000000000000 ) ) ;
#16204 = CARTESIAN_POINT ( 'NONE',  ( 2.002547531651519996, -7.942910686618100513, -9.778737580845787036 ) ) ;
#16205 = ADVANCED_FACE ( 'NONE', ( #4051 ), #9717, .F. ) ;
#16206 = VECTOR ( 'NONE', #16607, 1000.000000000000114 ) ;
#16207 = DIRECTION ( 'NONE',  ( -0.7635533937278214944, 0.2197766120036462600, 0.6071939193889586139 ) ) ;
#16208 = CARTESIAN_POINT ( 'NONE',  ( 16.58200780006414732, -0.0006320991582339893951, -0.01115192838421470191 ) ) ;
#16209 = B_SPLINE_CURVE_WITH_KNOTS ( 'NONE', 3,
 ( #9478, #9389, #13777, #15216, #689, #3735 ),
 .UNSPECIFIED., .F., .F.,
 ( 4, 2, 4 ),
 ( 0.000000000000000000, 0.0001828790815886945087, 0.0003657581631773890174 ),
 .UNSPECIFIED. ) ;
#16210 = ORIENTED_EDGE ( 'NONE', *, *, #14176, .F. ) ;
#16211 = EDGE_LOOP ( 'NONE', ( #17374, #6708, #6514, #8659 ) ) ;
#16212 = EDGE_LOOP ( 'NONE', ( #12657, #17844, #13047, #11909 ) ) ;
#16213 = B_SPLINE_CURVE_WITH_KNOTS ( 'NONE', 3,
 ( #4572, #5996, #11925, #17763, #11835, #13162, #75, #9058, #17672, #16132, #4667, #11736, #273 ),
 .UNSPECIFIED., .F., .F.,
 ( 4, 3, 3, 3, 4 ),
 ( 4.906538933386797396E-18, 0.0002299780670421066068, 0.0004599561239687925598, 0.0006896788984287864372, 0.0009194956271626387621 ),
 .UNSPECIFIED. ) ;
#16214 = VERTEX_POINT ( 'NONE', #12746 ) ;
#16215 = CARTESIAN_POINT ( 'NONE',  ( 2.705023505549864371, 4.909285963184069956, 12.36217802824807421 ) ) ;
#16216 = CARTESIAN_POINT ( 'NONE',  ( 16.56753206892534891, -0.008490833999798953410, -0.004253784598196148035 ) ) ;
#16217 = DIRECTION ( 'NONE',  ( -1.000000000000000000, 0.000000000000000000, 0.000000000000000000 ) ) ;
#16218 = EDGE_LOOP ( 'NONE', ( #9374, #17105, #11514, #4910 ) ) ;
#16219 = LINE ( 'NONE', #8947, #4734 ) ;
#16220 = CARTESIAN_POINT ( 'NONE',  ( 1.845756295923360435, -12.43231724724606835, 0.4783934145701590479 ) ) ;
#16221 = CIRCLE ( 'NONE', #4323, 5.000000000000000888 ) ;
#16222 = CARTESIAN_POINT ( 'NONE',  ( 16.56872352241294521, 0.007512283835805451566, 0.007240717549634016065 ) ) ;
#16223 = MANIFOLD_SOLID_BREP ( 'Keyway', #15477 ) ;
#16224 = CARTESIAN_POINT ( 'NONE',  ( 0.3720661004400040439, -4.951033743989553315, -12.89739157014198057 ) ) ;
#16225 = CARTESIAN_POINT ( 'NONE',  ( 0.3137051932979757485, 8.442169467526850823, 10.83767969834806166 ) ) ;
#16226 = ADVANCED_FACE ( 'NONE', ( #7214 ), #10221, .F. ) ;
#16227 = CARTESIAN_POINT ( 'NONE',  ( 1.847372867223030068, 11.86627781945713167, -3.744745203533853317 ) ) ;
#16228 = CARTESIAN_POINT ( 'NONE',  ( 1.959212340397916030, 9.750290364083625150, 7.909199412631181758 ) ) ;
#16229 = DIRECTION ( 'NONE',  ( -1.000000000000000000, 0.000000000000000000, 0.000000000000000000 ) ) ;
#16230 = B_SPLINE_CURVE_WITH_KNOTS ( 'NONE', 3,
 ( #1907, #4868, #18146, #5046, #10898, #752 ),
 .UNSPECIFIED., .F., .F.,
 ( 4, 2, 4 ),
 ( 0.000000000000000000, 0.001656992708824547161, 0.003313985417649093455 ),
 .UNSPECIFIED. ) ;
#16231 = CARTESIAN_POINT ( 'NONE',  ( -4.999999999999995559, -30.00000000000000000, 6.000000000000000000 ) ) ;
#16232 = EDGE_CURVE ( 'NONE', #1343, #10403, #4139, .T. ) ;
#16233 = ORIENTED_EDGE ( 'NONE', *, *, #17987, .T. ) ;
#16234 = PRODUCT ( 'gear driver shaft', 'gear driver shaft', '', ( #8174 ) ) ;
#16235 = ORIENTED_EDGE ( 'NONE', *, *, #18762, .F. ) ;
#16236 = ORIENTED_EDGE ( 'NONE', *, *, #11938, .F. ) ;
#16237 = VERTEX_POINT ( 'NONE', #15800 ) ;
#16238 = DIRECTION ( 'NONE',  ( 0.000000000000000000, 0.000000000000000000, 1.000000000000000000 ) ) ;
#16239 = ORIENTED_EDGE ( 'NONE', *, *, #8715, .F. ) ;
#16240 = CARTESIAN_POINT ( 'NONE',  ( 0.4862570985993235340, 8.769551628660890330, -10.79774104611363761 ) ) ;
#16241 = FACE_OUTER_BOUND ( 'NONE', #17285, .T. ) ;
#16242 = CARTESIAN_POINT ( 'NONE',  ( 2.353870697619111940, 10.00946331859664085, 8.216087327472971324 ) ) ;
#16243 = AXIS2_PLACEMENT_3D ( 'NONE', #8422, #7286, #15675 ) ;
#16244 = CARTESIAN_POINT ( 'NONE',  ( 3.074695600507531434, 11.23985886659412259, 10.75417554975680900 ) ) ;
#16245 = EDGE_LOOP ( 'NONE', ( #4722, #9492, #14712, #18709, #7425, #18682, #8110, #3800, #11093, #12541, #5090, #11029, #5188, #5681, #7523, #9821, #7365, #4010, #7011, #17036, #5979, #6220, #445, #2250, #14964, #13904, #5831, #15339, #14871, #16312, #15523, #15194, #12207, #15160, #6871, #13456, #9549, #7064, #4382, #3350, #9918, #17746, #11648, #2898, #10621, #15457, #4520, #4182, #18738, #6874, #2896, #2578, #15627, #4578, #8254, #3772, #14332, #15541, #3731, #9309, #1298, #18730, #2166, #3416 ) ) ;
#16246 = CARTESIAN_POINT ( 'NONE',  ( -0.3448739086965367795, 7.500000000000000000, -14.22069309503974921 ) ) ;
#16247 = CARTESIAN_POINT ( 'NONE',  ( -0.2192422490275049152, -45.00000000000000000, 3.000000000000000000 ) ) ;
#16248 = CARTESIAN_POINT ( 'NONE',  ( -6.500524771654098366, 7.499999999999099387, -12.09892167832694199 ) ) ;
#16249 = FACE_OUTER_BOUND ( 'NONE', #17328, .T. ) ;
#16250 = B_SPLINE_CURVE_WITH_KNOTS ( 'NONE', 3,
 ( #10727, #405, #14829, #16272, #4805, #7483 ),
 .UNSPECIFIED., .F., .F.,
 ( 4, 2, 4 ),
 ( 8.673617379884035472E-19, 0.0001828790815886939666, 0.0003657581631773870658 ),
 .UNSPECIFIED. ) ;
#16251 = CARTESIAN_POINT ( 'NONE',  ( 2.320520222536399668, 3.126729907239529815, 15.43440824796666710 ) ) ;
#16252 = CARTESIAN_POINT ( 'NONE',  ( 0.3137051932979792457, 12.91601973349270871, 4.679953077377533965 ) ) ;
#16253 = EDGE_CURVE ( 'NONE', #12855, #12290, #3905, .T. ) ;
#16254 = CARTESIAN_POINT ( 'NONE',  ( 0.3095370825347224519, -7.700448427571790155, -11.38092634279636961 ) ) ;
#16255 = EDGE_CURVE ( 'NONE', #7527, #10168, #2785, .T. ) ;
#16256 = ADVANCED_FACE ( 'NONE', ( #1271 ), #3241, .F. ) ;
#16257 = VERTEX_POINT ( 'NONE', #15519 ) ;
#16258 = AXIS2_PLACEMENT_3D ( 'NONE', #15233, #18285, #4917 ) ;
#16259 = CARTESIAN_POINT ( 'NONE',  ( 3.377929128793397684, -10.50432311212909475, 9.234024516648283054 ) ) ;
#16261 = ORIENTED_EDGE ( 'NONE', *, *, #11124, .F. ) ;
#16260 = DIRECTION ( 'NONE',  ( -1.000000000000000000, -0.000000000000000000, -0.000000000000000000 ) ) ;
#16262 = CARTESIAN_POINT ( 'NONE',  ( 3.664313757352974932, -5.926151963190458893, 12.97355833021538096 ) ) ;
#16263 = CARTESIAN_POINT ( 'NONE',  ( -66.35602477868047799, -10.00000000000000888, 5.999999999999999112 ) ) ;
#16264 = ORIENTED_EDGE ( 'NONE', *, *, #16911, .T. ) ;
#16265 = DIRECTION ( 'NONE',  ( -1.540743955509788340E-33, -1.000000000000000000, -2.533398541561209262E-17 ) ) ;
#16266 = UNCERTAINTY_MEASURE_WITH_UNIT (LENGTH_MEASURE( 1.000000000000000082E-05 ), #6264, 'distance_accuracy_value', 'NONE');
#16267 = B_SPLINE_CURVE_WITH_KNOTS ( 'NONE', 3,
 ( #5185, #6811, #11030, #16847 ),
 .UNSPECIFIED., .F., .F.,
 ( 4, 4 ),
 ( 0.000000000000000000, 0.002004993803842541195 ),
 .UNSPECIFIED. ) ;
#16268 = DIRECTION ( 'NONE',  ( -1.000000000000000000, 0.000000000000000000, 0.000000000000000000 ) ) ;
#16269 = ORIENTED_EDGE ( 'NONE', *, *, #4663, .T. ) ;
#16270 = CARTESIAN_POINT ( 'NONE',  ( 1.846524061778021419, 4.180439405448487911, -11.71897913237544664 ) ) ;
#16271 = CARTESIAN_POINT ( 'NONE',  ( 0.4754618798421167414, -13.89949764182682124, -0.7484603771385852644 ) ) ;
#16272 = CARTESIAN_POINT ( 'NONE',  ( 1.918921323896324083, 11.69058285425790977, 4.466082741316246718 ) ) ;
#16273 = CARTESIAN_POINT ( 'NONE',  ( 16.57210152137263393, -0.008007331252332796495, -0.01214401161737526519 ) ) ;
#16274 = ORIENTED_EDGE ( 'NONE', *, *, #15840, .T. ) ;
#16275 = B_SPLINE_CURVE_WITH_KNOTS ( 'NONE', 3,
 ( #2907, #7142, #2634, #11445 ),
 .UNSPECIFIED., .F., .F.,
 ( 4, 4 ),
 ( 2.076240083260000355E-17, 0.003005512676784849197 ),
 .UNSPECIFIED. ) ;
#16276 = AXIS2_PLACEMENT_3D ( 'NONE', #18583, #11337, #12570 ) ;
#16277 = CARTESIAN_POINT ( 'NONE',  ( 8.522092701127531811, 6.489356537178224471, -2.505958102592553693 ) ) ;
#16278 = CARTESIAN_POINT ( 'NONE',  ( 3.074695600507405757, 7.366518011945858646, 13.70113613813188458 ) ) ;
#16279 = ADVANCED_FACE ( 'NONE', ( #8272 ), #5680, .F. ) ;
#16280 =( BOUNDED_SURFACE ( )  B_SPLINE_SURFACE ( 3, 1, ( 
 ( #10085, #11253 ),
 ( #2620, #8649 ),
 ( #1008, #8558 ),
 ( #18403, #8469 ) ),
 .UNSPECIFIED., .F., .F., .T. ) 
 B_SPLINE_SURFACE_WITH_KNOTS ( ( 4, 4 ),
 ( 2, 2 ),
 ( 0.000000000000000000, 1.000000000000000000 ),
 ( 0.000000000000000000, 1.000000000000000000 ),
 .UNSPECIFIED. ) 
 GEOMETRIC_REPRESENTATION_ITEM ( )  RATIONAL_B_SPLINE_SURFACE ( (
 ( 1.000000000000000000, 1.000000000000000000),
 ( 0.7792777138730158093, 0.9689936506012928330),
 ( 0.7792777138730158093, 0.9689936506012928330),
 ( 1.000000000000000000, 1.000000000000000000) ) ) 
 REPRESENTATION_ITEM ( '' )  SURFACE ( )  );
#16281 = CARTESIAN_POINT ( 'NONE',  ( 16.58200780006414732, 0.009393638146078525306, 0.006043560077721743008 ) ) ;
#16282 = CARTESIAN_POINT ( 'NONE',  ( -110.4113270445337918, -81.60345299795268659, -91.28051051278382033 ) ) ;
#16283 = EDGE_CURVE ( 'NONE', #6964, #5564, #17723, .T. ) ;
#16284 = VERTEX_POINT ( 'NONE', #3066 ) ;
#16285 = DIRECTION ( 'NONE',  ( 0.000000000000000000, 0.000000000000000000, 1.000000000000000000 ) ) ;
#16286 = CARTESIAN_POINT ( 'NONE',  ( 2.002547531651519996, 12.17374746633578475, 3.242439124566693476 ) ) ;
#16287 = VERTEX_POINT ( 'NONE', #13312 ) ;
#16288 = ORIENTED_EDGE ( 'NONE', *, *, #5563, .F. ) ;
#16289 = CARTESIAN_POINT ( 'NONE',  ( 1.474209205587600965E-14, -8.013167318348353163, 37.51316734529530805 ) ) ;
#16290 = ORIENTED_EDGE ( 'NONE', *, *, #4349, .T. ) ;
#16291 = CARTESIAN_POINT ( 'NONE',  ( 1.342453679581834924, 11.38190519890853558, 9.456403821038842139 ) ) ;
#16292 = VERTEX_POINT ( 'NONE', #11792 ) ;
#16293 = EDGE_CURVE ( 'NONE', #11007, #620, #8245, .T. ) ;
#16294 = VECTOR ( 'NONE', #15127, 1000.000000000000227 ) ;
#16295 = AXIS2_PLACEMENT_3D ( 'NONE', #5499, #14211, #18504 ) ;
#16296 = CARTESIAN_POINT ( 'NONE',  ( 2.002547531651519996, 6.845637710436341727, -10.57595306287284842 ) ) ;
#16297 = CARTESIAN_POINT ( 'NONE',  ( 0.3145729642390355796, -13.73540280162741212, 0.3065092323350734893 ) ) ;
#16298 = CARTESIAN_POINT ( 'NONE',  ( 1.977228804421385933, 15.33060379559031539, -1.488378900181928532 ) ) ;
#16299 = CARTESIAN_POINT ( 'NONE',  ( 0.4385251269669947494, -13.39302348765811068, 3.577373010348662508 ) ) ;
#16300 = PLANE ( 'NONE',  #10225 ) ;
#16301 = CARTESIAN_POINT ( 'NONE',  ( 16.56782317627811096, 0.009228812961908652857, -0.003357783021327854014 ) ) ;
#16302 = SURFACE_STYLE_USAGE ( .BOTH. , #13424 ) ;
#16303 = FACE_OUTER_BOUND ( 'NONE', #4073, .T. ) ;
#16304 = CARTESIAN_POINT ( 'NONE',  ( 2.002547531651519996, 4.532360870844327039, 11.75462648437103752 ) ) ;
#16305 = CARTESIAN_POINT ( 'NONE',  ( 16.56679352167444819, 0.006526964904752344775, -0.006618561353600113835 ) ) ;
#16306 = LINE ( 'NONE', #13429, #2929 ) ;
#16307 = CIRCLE ( 'NONE', #18725, 5.000000000000000000 ) ;
#16308 = AXIS2_PLACEMENT_3D ( 'NONE', #762, #10907, #18335 ) ;
#16309 = EDGE_CURVE ( 'NONE', #6378, #322, #13934, .T. ) ;
#16310 = DIRECTION ( 'NONE',  ( 1.000000000000000000, 0.000000000000000000, 0.000000000000000000 ) ) ;
#16311 = LINE ( 'NONE', #3490, #5673 ) ;
#16312 = ORIENTED_EDGE ( 'NONE', *, *, #12285, .F. ) ;
#16313 = VERTEX_POINT ( 'NONE', #16091 ) ;
#16314 = ORIENTED_EDGE ( 'NONE', *, *, #12311, .F. ) ;
#16315 = ORIENTED_EDGE ( 'NONE', *, *, #12668, .F. ) ;
#16316 = CARTESIAN_POINT ( 'NONE',  ( 2.002547531651519996, -12.57989064830759141, -0.6781519942173057647 ) ) ;
#16317 = FACE_OUTER_BOUND ( 'NONE', #6343, .T. ) ;
#16318 =( BOUNDED_SURFACE ( )  B_SPLINE_SURFACE ( 3, 1, ( 
 ( #14498, #11359 ),
 ( #15929, #5693 ),
 ( #14314, #5888 ),
 ( #15835, #17464 ) ),
 .UNSPECIFIED., .F., .F., .T. ) 
 B_SPLINE_SURFACE_WITH_KNOTS ( ( 4, 4 ),
 ( 2, 2 ),
 ( 0.000000000000000000, 1.000000000000000000 ),
 ( 0.000000000000000000, 1.000000000000000000 ),
 .UNSPECIFIED. ) 
 GEOMETRIC_REPRESENTATION_ITEM ( )  RATIONAL_B_SPLINE_SURFACE ( (
 ( 1.000000000000000000, 1.000000000000000000),
 ( 0.9933953342250436691, 0.8357391271907733676),
 ( 0.9933953342250436691, 0.8357391271907733676),
 ( 1.000000000000000000, 1.000000000000000000) ) ) 
 REPRESENTATION_ITEM ( '' )  SURFACE ( )  );
#16319 = CARTESIAN_POINT ( 'NONE',  ( 1.847412631396504468, -12.44294644888238821, -0.04315047898448168967 ) ) ;
#16320 = ORIENTED_EDGE ( 'NONE', *, *, #4987, .T. ) ;
#16321 = CARTESIAN_POINT ( 'NONE',  ( 0.3137051932979792457, -10.83767969834809008, 8.442169467526815296 ) ) ;
#16322 = CARTESIAN_POINT ( 'NONE',  ( 2.002547531651519996, 9.778737580845815458, -7.942910686618064986 ) ) ;
#16323 = VECTOR ( 'NONE', #13403, 1000.000000000000000 ) ;
#16324 = ORIENTED_EDGE ( 'NONE', *, *, #6731, .F. ) ;
#16325 = FACE_OUTER_BOUND ( 'NONE', #5437, .T. ) ;
#16326 = CARTESIAN_POINT ( 'NONE',  ( 1.847168016377980670, 12.44137401948661470, -0.1868244120189998803 ) ) ;
#16327 = B_SPLINE_CURVE_WITH_KNOTS ( 'NONE', 3,
 ( #6892, #17486, #7275, #13088, #18821, #18543, #11570, #3491, #5815, #14614, #4391, #10222, #4213 ),
 .UNSPECIFIED., .F., .F.,
 ( 4, 3, 3, 3, 4 ),
 ( 2.168404344971008868E-18, 0.0002299804304191468746, 0.0004599608082120234371, 0.0006467586077648000654, 0.0008336169836825981817 ),
 .UNSPECIFIED. ) ;
#16328 = CARTESIAN_POINT ( 'NONE',  ( 1.847421816787903071, 0.02876707915197697710, -12.44300551404155364 ) ) ;
#16329 = DIRECTION ( 'NONE',  ( -0.7635533937278216055, -0.6453904417649388714, 0.02138673900301666167 ) ) ;
#16330 = DIRECTION ( 'NONE',  ( -1.000000000000000000, 0.000000000000000000, -0.000000000000000000 ) ) ;
#16331 = CARTESIAN_POINT ( 'NONE',  ( 2.775557561562891351E-14, -16.57596421305226997, 25.01316731834833718 ) ) ;
#16332 = CARTESIAN_POINT ( 'NONE',  ( 20.00000000000000000, -2.500000000000000444, -16.99999999999999645 ) ) ;
#16333 = ORIENTED_EDGE ( 'NONE', *, *, #11407, .F. ) ;
#16334 = EDGE_LOOP ( 'NONE', ( #17594, #3681, #18861, #15965 ) ) ;
#16335 = AXIS2_PLACEMENT_3D ( 'NONE', #17580, #9928, #4494 ) ;
#16336 = EDGE_LOOP ( 'NONE', ( #10087, #2118, #8851, #7793, #8291, #8915, #4451, #15974, #16359, #5135, #6982 ) ) ;
#16337 = VERTEX_POINT ( 'NONE', #1559 ) ;
#16338 = VECTOR ( 'NONE', #14808, 1000.000000000000000 ) ;
#16339 = CARTESIAN_POINT ( 'NONE',  ( 1.847168016377979116, -7.464000291196340342, -9.955470380986712442 ) ) ;
#16340 = AXIS2_PLACEMENT_3D ( 'NONE', #12358, #5095, #2051 ) ;
#16341 = EDGE_CURVE ( 'NONE', #5432, #14483, #15305, .T. ) ;
#16342 = CARTESIAN_POINT ( 'NONE',  ( 3.353306896162453477, -10.44017738170049903, -9.252610477110389198 ) ) ;
#16343 = FACE_OUTER_BOUND ( 'NONE', #5466, .T. ) ;
#16344 = CARTESIAN_POINT ( 'NONE',  ( 16.58200780006414732, 0.002844973367391037070, 0.01080144354108989249 ) ) ;
#16345 = DIRECTION ( 'NONE',  ( 0.7561779333270775005, -0.2350349629540270657, 0.6106991889125030770 ) ) ;
#16346 = VERTEX_POINT ( 'NONE', #10551 ) ;
#16347 = CARTESIAN_POINT ( 'NONE',  ( 1.823557580623806018, 7.500000000000000888, -15.12114310604040313 ) ) ;
#16348 = DIRECTION ( 'NONE',  ( -0.000000000000000000, 1.000000000000000000, 0.000000000000000000 ) ) ;
#16349 = CARTESIAN_POINT ( 'NONE',  ( 2.747332970342022840, 2.409922051470680060, 16.17136872824899285 ) ) ;
#16350 = FACE_OUTER_BOUND ( 'NONE', #9716, .T. ) ;
#16351 = CARTESIAN_POINT ( 'NONE',  ( -194.9999999999999716, -30.00000000000003197, 0.000000000000000000 ) ) ;
#16352 = LINE ( 'NONE', #9083, #14418 ) ;
#16353 = CIRCLE ( 'NONE', #12065, 5.000000000000000000 ) ;
#16354 = CIRCLE ( 'NONE', #7515, 5.000000000000000000 ) ;
#16355 = CARTESIAN_POINT ( 'NONE',  ( 0.4862570985993235340, -10.79774104611379215, 8.769551628660700260 ) ) ;
#16356 = ORIENTED_EDGE ( 'NONE', *, *, #17461, .F. ) ;
#16357 = CARTESIAN_POINT ( 'NONE',  ( 0.4862570985993235340, 8.769551628660735787, 10.79774104611376373 ) ) ;
#16359 = ORIENTED_EDGE ( 'NONE', *, *, #15368, .T. ) ;
#16358 = DIRECTION ( 'NONE',  ( -1.000000000000000000, -0.000000000000000000, -0.000000000000000000 ) ) ;
#16360 = CARTESIAN_POINT ( 'NONE',  ( 0.4384471787762856398, 11.63197976518328680, 7.540925784514595165 ) ) ;
#16361 = B_SPLINE_CURVE_WITH_KNOTS ( 'NONE', 3,
 ( #7826, #12115, #15067, #6185 ),
 .UNSPECIFIED., .F., .F.,
 ( 4, 4 ),
 ( 0.000000000000000000, 0.002004993803842800969 ),
 .UNSPECIFIED. ) ;
#16362 = ORIENTED_EDGE ( 'NONE', *, *, #6620, .T. ) ;
#16363 = LINE ( 'NONE', #17497, #15323 ) ;
#16364 = ORIENTED_EDGE ( 'NONE', *, *, #6009, .F. ) ;
#16365 = CARTESIAN_POINT ( 'NONE',  ( 1.104287921197080512E-14, -7.013167318348350499, 25.01316734529528674 ) ) ;
#16366 = AXIS2_PLACEMENT_3D ( 'NONE', #11288, #15235, #5525 ) ;
#16367 = CARTESIAN_POINT ( 'NONE',  ( 6.021941181548189803, -3.575661417670232822, -12.00000000127650246 ) ) ;
#16368 = VERTEX_POINT ( 'NONE', #8822 ) ;
#16369 = LINE ( 'NONE', #3252, #10282 ) ;
#16370 = ADVANCED_FACE ( 'NONE', ( #16384 ), #13013, .T. ) ;
#16371 = CARTESIAN_POINT ( 'NONE',  ( 0.3137051932979792457, 13.73004976592202198, 0.4596302728640249136 ) ) ;
#16372 = CYLINDRICAL_SURFACE ( 'NONE', #5203, 5.000000000000000000 ) ;
#16373 = CARTESIAN_POINT ( 'NONE',  ( 0.000000000000000000, 0.000000000000000000, -13.00000000000000533 ) ) ;
#16374 = ORIENTED_EDGE ( 'NONE', *, *, #645, .F. ) ;
#16375 = CARTESIAN_POINT ( 'NONE',  ( 0.4862570985993235340, -10.79774104611366781, -8.769551628660854803 ) ) ;
#16376 = CARTESIAN_POINT ( 'NONE',  ( 0.3151930723728406103, 11.07033375389132246, 8.137566970826403789 ) ) ;
#16377 = VECTOR ( 'NONE', #14111, 1000.000000000000000 ) ;
#16378 =( GEOMETRIC_REPRESENTATION_CONTEXT ( 3 ) GLOBAL_UNCERTAINTY_ASSIGNED_CONTEXT ( ( #14754 ) ) GLOBAL_UNIT_ASSIGNED_CONTEXT ( ( #15885, #13205, #694 ) ) REPRESENTATION_CONTEXT ( 'NONE', 'WORKASPACE' ) );
#16379 = CARTESIAN_POINT ( 'NONE',  ( 0.3137051932979792457, 13.20008686438105983, 3.805684345189833451 ) ) ;
#16380 = CARTESIAN_POINT ( 'NONE',  ( 1.560000000000000053, 0.8660254037844389297, 1.500000000000000000 ) ) ;
#16381 = FACE_OUTER_BOUND ( 'NONE', #16115, .T. ) ;
#16382 = EDGE_LOOP ( 'NONE', ( #6083, #276, #8203, #10745 ) ) ;
#16383 = CARTESIAN_POINT ( 'NONE',  ( 0.3137051932979809665, 3.805684345189785933, 13.20008686438107581 ) ) ;
#16384 = FACE_OUTER_BOUND ( 'NONE', #3094, .T. ) ;
#16385 = ORIENTED_EDGE ( 'NONE', *, *, #17542, .T. ) ;
#16386 = ORIENTED_EDGE ( 'NONE', *, *, #9263, .F. ) ;
#16387 = DIRECTION ( 'NONE',  ( -0.000000000000000000, 0.000000000000000000, -1.000000000000000000 ) ) ;
#16388 = VERTEX_POINT ( 'NONE', #14555 ) ;
#16389 = CARTESIAN_POINT ( 'NONE',  ( 1.845755665166726844, 3.386720041070728104, 11.97169564665392727 ) ) ;
#16390 = EDGE_LOOP ( 'NONE', ( #13608, #10162, #17962, #3374 ) ) ;
#16391 = ADVANCED_FACE ( 'NONE', ( #1756 ), #1177, .F. ) ;
#16392 = EDGE_CURVE ( 'NONE', #2855, #7766, #5750, .T. ) ;
#16393 = AXIS2_PLACEMENT_3D ( 'NONE', #2423, #6927, #7110 ) ;
#16394 = EDGE_CURVE ( 'NONE', #15610, #18169, #15174, .T. ) ;
#16395 = CARTESIAN_POINT ( 'NONE',  ( 2.002547531651520885, 10.57595306287292480, 6.845637710436228929 ) ) ;
#16396 = PRESENTATION_STYLE_ASSIGNMENT (( #3076 ) ) ;
#16397 = CARTESIAN_POINT ( 'NONE',  ( 0.3137051932979757485, 13.73004976592202020, -0.4596302728640235258 ) ) ;
#16398 = CARTESIAN_POINT ( 'NONE',  ( 0.3308579732647007887, -8.558831104906994725, 10.76782854710824111 ) ) ;
#16399 = B_SPLINE_CURVE_WITH_KNOTS ( 'NONE', 3,
 ( #7782, #7973, #18184, #2136, #13595, #18091 ),
 .UNSPECIFIED., .F., .F.,
 ( 4, 2, 4 ),
 ( 0.000000000000000000, 0.0001828790815886950779, 0.0003657581631773901558 ),
 .UNSPECIFIED. ) ;
#16400 = CIRCLE ( 'NONE', #14855, 14.54644660717763927 ) ;
#16401 = CARTESIAN_POINT ( 'NONE',  ( 0.3132642857406554571, 12.89240536501346313, 4.743831191224429311 ) ) ;
#16402 = CARTESIAN_POINT ( 'NONE',  ( 0.3058872367615226295, -3.664492643742672584, -13.24582953854928569 ) ) ;
#16403 =( BOUNDED_SURFACE ( )  B_SPLINE_SURFACE ( 3, 1, ( 
 ( #5995, #11639 ),
 ( #7642, #7350 ),
 ( #10199, #11833 ),
 ( #8957, #4373 ) ),
 .UNSPECIFIED., .F., .F., .T. ) 
 B_SPLINE_SURFACE_WITH_KNOTS ( ( 4, 4 ),
 ( 2, 2 ),
 ( 0.000000000000000000, 1.000000000000000000 ),
 ( 0.000000000000000000, 1.000000000000000000 ),
 .UNSPECIFIED. ) 
 GEOMETRIC_REPRESENTATION_ITEM ( )  RATIONAL_B_SPLINE_SURFACE ( (
 ( 1.000000000000000000, 1.000000000000000000),
 ( 0.9933953342250438912, 0.8357391271907739227),
 ( 0.9933953342250438912, 0.8357391271907739227),
 ( 1.000000000000000000, 1.000000000000000000) ) ) 
 REPRESENTATION_ITEM ( '' )  SURFACE ( )  );
#16404 =( LENGTH_UNIT ( ) NAMED_UNIT ( * ) SI_UNIT ( .MILLI., .METRE. ) );
#16405 = CARTESIAN_POINT ( 'NONE',  ( 0.3137051932979757485, 8.442169467526850823, 10.83767969834806166 ) ) ;
#16406 = CARTESIAN_POINT ( 'NONE',  ( 0.4862570985993235340, -11.67702470553370553, 7.559321496869385371 ) ) ;
#16407 = CIRCLE ( 'NONE', #524, 16.06066017081991149 ) ;
#16408 = DIRECTION ( 'NONE',  ( 0.000000000000000000, 0.000000000000000000, -1.000000000000000000 ) ) ;
#16409 = AXIS2_PLACEMENT_3D ( 'NONE', #13163, #13740, #15179 ) ;
#16410 = CARTESIAN_POINT ( 'NONE',  ( 0.3939822652208094800, -7.545099438011941828, -11.57634296752776137 ) ) ;
#16411 = AXIS2_PLACEMENT_3D ( 'NONE', #9400, #3368, #18281 ) ;
#16412 = CLOSED_SHELL ( 'NONE', ( #17664, #16142, #10568, #11070, #9797, #7453, #5370, #6747, #9161, #15369, #10131, #5835, #18572, #14383, #1567, #15852, #13418, #6466, #11460, #17299, #11459, #3951, #8542, #6701, #13179, #7474, #15817 ) ) ;
#16413 = DIRECTION ( 'NONE',  ( 0.7561779333270775005, -0.5081796452863246438, -0.4122479608995723299 ) ) ;
#16414 = CARTESIAN_POINT ( 'NONE',  ( 16.56872352241294521, -0.001442253899401298341, 0.01033355228142499027 ) ) ;
#16415 = ORIENTED_EDGE ( 'NONE', *, *, #747, .F. ) ;
#16416 = ORIENTED_EDGE ( 'NONE', *, *, #8668, .F. ) ;
#16417 = VERTEX_POINT ( 'NONE', #10352 ) ;
#16418 = ORIENTED_EDGE ( 'NONE', *, *, #586, .T. ) ;
#16419 = CARTESIAN_POINT ( 'NONE',  ( 0.3151926232592474064, 0.07678256780557664307, 13.73922722301401578 ) ) ;
#16420 = CARTESIAN_POINT ( 'NONE',  ( 0.3137051932979809665, 10.83767969834803324, 8.442169467526891680 ) ) ;
#16421 = CARTESIAN_POINT ( 'NONE',  ( -30.00000000000000355, -12.50000000000000178, 6.000000000000000000 ) ) ;
#16422 = CARTESIAN_POINT ( 'NONE',  ( 3.950837973638677170, 1.958075594453790869, 14.41405733518061538 ) ) ;
#16423 = DIRECTION ( 'NONE',  ( 0.000000000000000000, -1.000000000000000000, 0.000000000000000000 ) ) ;
#16424 = ADVANCED_FACE ( 'NONE', ( #8913 ), #17532, .F. ) ;
#16425 = FACE_OUTER_BOUND ( 'NONE', #4055, .T. ) ;
#16426 = LINE ( 'NONE', #18128, #7989 ) ;
#16427 = CARTESIAN_POINT ( 'NONE',  ( 0.3137051932979792457, 7.698472063774471685, 11.37800749014133928 ) ) ;
#16428 = DIRECTION ( 'NONE',  ( 0.000000000000000000, 0.000000000000000000, -1.000000000000000000 ) ) ;
#16429 = CARTESIAN_POINT ( 'NONE',  ( 2.320521194581854907, 10.64885423995017355, 11.60169518685927059 ) ) ;
#16430 = DIRECTION ( 'NONE',  ( 0.000000000000000000, 0.000000000000000000, -1.000000000000000000 ) ) ;
#16431 = DIRECTION ( 'NONE',  ( 1.000000000000000000, 0.000000000000000000, 0.000000000000000000 ) ) ;
#16432 = CARTESIAN_POINT ( 'NONE',  ( 0.3137051932979757485, -8.442169467526770887, -10.83767969834812561 ) ) ;
#16433 = VECTOR ( 'NONE', #14980, 1000.000000000000000 ) ;
#16434 = EDGE_LOOP ( 'NONE', ( #156, #2366, #11367, #10045 ) ) ;
#16435 = ORIENTED_EDGE ( 'NONE', *, *, #1715, .T. ) ;
#16436 = ORIENTED_EDGE ( 'NONE', *, *, #8965, .T. ) ;
#16437 = ORIENTED_EDGE ( 'NONE', *, *, #1398, .F. ) ;
#16438 = CARTESIAN_POINT ( 'NONE',  ( -30.00000000000000355, -12.50000000000000178, 6.000000000000000000 ) ) ;
#16439 = CARTESIAN_POINT ( 'NONE',  ( 2.002547531651519996, -9.778737580845639599, -7.942910686618280813 ) ) ;
#16440 = B_SPLINE_CURVE_WITH_KNOTS ( 'NONE', 3,
 ( #2793, #7318, #1482, #8550, #18768, #18579 ),
 .UNSPECIFIED., .F., .F.,
 ( 4, 2, 4 ),
 ( 8.131516293641283255E-19, 0.001657017934709845109, 0.003314035869419688484 ),
 .UNSPECIFIED. ) ;
#16441 = CARTESIAN_POINT ( 'NONE',  ( 20.00000000000000711, -40.00000000000000000, 6.000000000000000000 ) ) ;
#16442 = CARTESIAN_POINT ( 'NONE',  ( 2.636624412716062071, -14.14563173255412742, -7.605649742760987486 ) ) ;
#16443 = EDGE_CURVE ( 'NONE', #5049, #471, #14629, .T. ) ;
#16444 = CARTESIAN_POINT ( 'NONE',  ( 3.353306896162455697, 1.348936822033017124, -13.88482890973694950 ) ) ;
#16445 = ORIENTED_EDGE ( 'NONE', *, *, #8085, .F. ) ;
#16446 = CARTESIAN_POINT ( 'NONE',  ( -2.611515231136698034, 7.500000000000001776, -15.68397129924701794 ) ) ;
#16447 = AXIS2_PLACEMENT_3D ( 'NONE', #2455, #6974, #15559 ) ;
#16448 = CARTESIAN_POINT ( 'NONE',  ( 0.3095370825347234511, -7.700448427571787491, -11.38092634279637139 ) ) ;
#16449 = EDGE_CURVE ( 'NONE', #137, #11551, #2526, .T. ) ;
#16450 = CARTESIAN_POINT ( 'NONE',  ( 16.57778382496167424, 0.01092721432668994352, 0.01018821665058780926 ) ) ;
#16451 = CARTESIAN_POINT ( 'NONE',  ( 2.123976203522053741, -3.347755036806012274, 15.26039569100259108 ) ) ;
#16452 = B_SPLINE_CURVE_WITH_KNOTS ( 'NONE', 3,
 ( #4065, #12666, #9882, #7127, #14011, #9983 ),
 .UNSPECIFIED., .F., .F.,
 ( 4, 2, 4 ),
 ( 1.946286347258496500E-18, 0.0002017457492448080964, 0.0004034914984896142412 ),
 .UNSPECIFIED. ) ;
#16453 = CARTESIAN_POINT ( 'NONE',  ( 0.8740779401508622648, 0.8420120399581700887, 14.27348745891572968 ) ) ;
#16454 = CARTESIAN_POINT ( 'NONE',  ( 2.636624412715093513, -14.14563173255330142, 7.605649742761597665 ) ) ;
#16455 = VERTEX_POINT ( 'NONE', #11026 ) ;
#16456 = CARTESIAN_POINT ( 'NONE',  ( -66.35602477868049220, -15.00000000000001066, 5.999999999999999112 ) ) ;
#16458 = VERTEX_POINT ( 'NONE', #15135 ) ;
#16457 = FACE_OUTER_BOUND ( 'NONE', #14528, .T. ) ;
#16459 = DIRECTION ( 'NONE',  ( -0.7635533937278214944, 0.6071939193889607234, -0.2197766120036399873 ) ) ;
#16460 = EDGE_CURVE ( 'NONE', #4964, #10109, #16902, .T. ) ;
#16461 = CARTESIAN_POINT ( 'NONE',  ( 3.950837973638675393, 10.51028938476217967, 10.05648675950130233 ) ) ;
#16462 = VERTEX_POINT ( 'NONE', #6441 ) ;
#16463 = CARTESIAN_POINT ( 'NONE',  ( 3.950837973638675393, -6.888253895133384930, 12.81214529934972823 ) ) ;
#16464 = CARTESIAN_POINT ( 'NONE',  ( -1.329112640582302607, -6.875529660588494352, -12.00000000371739084 ) ) ;
#16465 = ORIENTED_EDGE ( 'NONE', *, *, #5347, .F. ) ;
#16466 = CARTESIAN_POINT ( 'NONE',  ( 3.664313757352975376, 9.645155442698909454, -10.50730552161222597 ) ) ;
#16467 = LINE ( 'NONE', #14828, #10674 ) ;
#16468 = CARTESIAN_POINT ( 'NONE',  ( 1.845755665166724846, 4.296872077620840891, -11.67596932341229987 ) ) ;
#16469 = DIRECTION ( 'NONE',  ( -0.000000000000000000, -0.000000000000000000, 1.000000000000000000 ) ) ;
#16470 = ORIENTED_EDGE ( 'NONE', *, *, #13673, .F. ) ;
#16471 = VECTOR ( 'NONE', #4706, 1000.000000000000227 ) ;
#16472 = AXIS2_PLACEMENT_3D ( 'NONE', #960, #17387, #2838 ) ;
#16473 = EDGE_CURVE ( 'NONE', #18879, #3494, #16844, .T. ) ;
#16474 = DIRECTION ( 'NONE',  ( -0.7561779333270775005, 0.6106991889125087392, -0.2350349629540122165 ) ) ;
#16475 = CARTESIAN_POINT ( 'NONE',  ( -3.335251384444446021, -19.99999999999999645, 3.000000000000000000 ) ) ;
#16476 = B_SPLINE_CURVE_WITH_KNOTS ( 'NONE', 3,
 ( #18325, #1109, #2630, #11348, #15360, #3796 ),
 .UNSPECIFIED., .F., .F.,
 ( 4, 2, 4 ),
 ( 1.939479807224432123E-18, 0.001500839035891553524, 0.003001678071783104879 ),
 .UNSPECIFIED. ) ;
#16477 = CARTESIAN_POINT ( 'NONE',  ( 0.4754618798421162973, 0.7484603771384427118, 13.89949764182683012 ) ) ;
#16479 = ORIENTED_EDGE ( 'NONE', *, *, #8264, .T. ) ;
#16478 = CARTESIAN_POINT ( 'NONE',  ( -30.00000000000000711, 20.00000000000000000, 3.000000000000000000 ) ) ;
#16480 = LINE ( 'NONE', #12078, #4198 ) ;
#16481 = COLOUR_RGB ( '', 0.09019608, 0.27058824, 0.51372549) ;
#16482 = ADVANCED_FACE ( 'NONE', ( #18189 ), #16923, .F. ) ;
#16483 = ORIENTED_EDGE ( 'NONE', *, *, #13154, .F. ) ;
#16484 = CARTESIAN_POINT ( 'NONE',  ( 0.3145734862173252822, -8.321353293018908914, 10.93207848441430130 ) ) ;
#16485 = DIRECTION ( 'NONE',  ( -0.7635533937278216055, 0.1790966170214010056, -0.6204116510013458763 ) ) ;
#16486 = EDGE_LOOP ( 'NONE', ( #4320, #6634, #2312, #17817 ) ) ;
#16487 = ORIENTED_EDGE ( 'NONE', *, *, #6275, .T. ) ;
#16488 = DIRECTION ( 'NONE',  ( -1.000000000000000000, -0.000000000000000000, -0.000000000000000000 ) ) ;
#16489 = CONICAL_SURFACE ( 'NONE', #17375, 14.54644660717763927, 0.8559913436420816257 ) ;
#16490 = VERTEX_POINT ( 'NONE', #10940 ) ;
#16491 = FACE_OUTER_BOUND ( 'NONE', #17161, .T. ) ;
#16492 = ORIENTED_EDGE ( 'NONE', *, *, #7282, .T. ) ;
#16493 = CARTESIAN_POINT ( 'NONE',  ( 0.3142014840576534684, 3.879477880151442015, 13.17932813834296013 ) ) ;
#16494 = CARTESIAN_POINT ( 'NONE',  ( 3.950837973638676281, -1.958075594453890789, 14.41405733518059940 ) ) ;
#16495 = CARTESIAN_POINT ( 'NONE',  ( 16.56872352241294521, -0.007512283835805501873, -0.007240717549633963156 ) ) ;
#16496 =( NAMED_UNIT ( * ) SI_UNIT ( $, .STERADIAN. ) SOLID_ANGLE_UNIT ( ) );
#16497 = CARTESIAN_POINT ( 'NONE',  ( 0.4754618798421171855, -5.007009103465158262, -12.98792082933649716 ) ) ;
#16498 = CARTESIAN_POINT ( 'NONE',  ( 2.353870697619110164, -3.268530966681543859, -12.53036919722787879 ) ) ;
#16499 = CARTESIAN_POINT ( 'NONE',  ( 0.3939875929385661668, 3.598491969338414531, -13.34133634968951831 ) ) ;
#16500 = CARTESIAN_POINT ( 'NONE',  ( 3.664313757352963830, 12.97355833021539873, 5.926151963190401162 ) ) ;
#16501 = EDGE_CURVE ( 'NONE', #3664, #14019, #10057, .T. ) ;
#16502 = EDGE_CURVE ( 'NONE', #9780, #14694, #5709, .T. ) ;
#16503 = ADVANCED_FACE ( 'NONE', ( #9300 ), #15312, .T. ) ;
#16504 = CARTESIAN_POINT ( 'NONE',  ( 16.56753206892534891, -0.006669401563384969034, 0.006760771273036147132 ) ) ;
#16505 = DIRECTION ( 'NONE',  ( 0.000000000000000000, 0.000000000000000000, 1.000000000000000000 ) ) ;
#16506 = ORIENTED_EDGE ( 'NONE', *, *, #221, .F. ) ;
#16507 = ORIENTED_EDGE ( 'NONE', *, *, #3184, .F. ) ;
#16508 = ORIENTED_EDGE ( 'NONE', *, *, #9354, .F. ) ;
#16509 = EDGE_LOOP ( 'NONE', ( #1585, #11344, #1911, #15752 ) ) ;
#16510 = CARTESIAN_POINT ( 'NONE',  ( 0.4862570985993252548, -5.003653737315580052, 12.97920246947877665 ) ) ;
#16511 = B_SPLINE_CURVE_WITH_KNOTS ( 'NONE', 3,
 ( #12980, #11286, #4103, #15656 ),
 .UNSPECIFIED., .F., .F.,
 ( 4, 4 ),
 ( 4.459867448574166155E-16, 0.002004993803842844771 ),
 .UNSPECIFIED. ) ;
#16512 = CARTESIAN_POINT ( 'NONE',  ( 2.002547531651519996, 12.17374746633582561, -3.242439124566524278 ) ) ;
#16513 = B_SPLINE_CURVE_WITH_KNOTS ( 'NONE', 3,
 ( #2072, #3487, #18207, #18025, #13898, #17938 ),
 .UNSPECIFIED., .F., .F.,
 ( 4, 2, 4 ),
 ( 0.000000000000000000, 0.001656992708822831520, 0.003313985417645663040 ),
 .UNSPECIFIED. ) ;
#16514 = CARTESIAN_POINT ( 'NONE',  ( 2.002547531651519996, -10.57595306287287329, -6.845637710436306200 ) ) ;
#16515 = EDGE_CURVE ( 'NONE', #17332, #913, #18006, .T. ) ;
#16516 =( BOUNDED_SURFACE ( )  B_SPLINE_SURFACE ( 3, 1, ( 
 ( #17776, #4490 ),
 ( #3027, #13557 ),
 ( #185, #6014 ),
 ( #16344, #1709 ) ),
 .UNSPECIFIED., .F., .F., .T. ) 
 B_SPLINE_SURFACE_WITH_KNOTS ( ( 4, 4 ),
 ( 2, 2 ),
 ( 0.000000000000000000, 1.000000000000000000 ),
 ( 0.000000000000000000, 1.000000000000000000 ),
 .UNSPECIFIED. ) 
 GEOMETRIC_REPRESENTATION_ITEM ( )  RATIONAL_B_SPLINE_SURFACE ( (
 ( 1.000000000000000000, 1.000000000000000000),
 ( 0.7792777138730160313, 0.9689936506012927220),
 ( 0.7792777138730160313, 0.9689936506012927220),
 ( 1.000000000000000000, 1.000000000000000000) ) ) 
 REPRESENTATION_ITEM ( '' )  SURFACE ( )  );
#16517 = CARTESIAN_POINT ( 'NONE',  ( 8.438534575730034959, 6.454982381540289360, 2.341351102130301065 ) ) ;
#16518 = CARTESIAN_POINT ( 'NONE',  ( 1.861706995891674099, -12.44571539481144384, 0.5394761475745415424 ) ) ;
#16519 = PRODUCT_DEFINITION_CONTEXT ( 'detailed design', #17423, 'design' ) ;
#16520 = ORIENTED_EDGE ( 'NONE', *, *, #4185, .F. ) ;
#16521 = DIRECTION ( 'NONE',  ( -1.000000000000000000, -0.000000000000000000, -0.000000000000000000 ) ) ;
#16522 = DIRECTION ( 'NONE',  ( -1.000000000000000000, -0.000000000000000000, -0.000000000000000000 ) ) ;
#16523 = CARTESIAN_POINT ( 'NONE',  ( 2.320521194583481606, -1.795798718314370213, -15.64520804578356561 ) ) ;
#16524 = DIRECTION ( 'NONE',  ( 0.000000000000000000, 0.000000000000000000, 1.000000000000000000 ) ) ;
#16525 = CARTESIAN_POINT ( 'NONE',  ( 1.861628059977341154, -11.66985327793196170, -4.358833901513171405 ) ) ;
#16526 = CARTESIAN_POINT ( 'NONE',  ( 0.3095370825347224519, -0.4597470195091133416, 13.73357284481724605 ) ) ;
#16527 = B_SPLINE_CURVE_WITH_KNOTS ( 'NONE', 3,
 ( #16919, #16828, #12608, #11198, #5353, #11290 ),
 .UNSPECIFIED., .F., .F.,
 ( 4, 2, 4 ),
 ( 0.000000000000000000, 0.001656992708824547161, 0.003313985417649093455 ),
 .UNSPECIFIED. ) ;
#16528 = CARTESIAN_POINT ( 'NONE',  ( 16.56753206892534891, 0.004253784598196760393, 0.008490833999798020129 ) ) ;
#16529 = ORIENTED_EDGE ( 'NONE', *, *, #15741, .F. ) ;
#16530 = ORIENTED_EDGE ( 'NONE', *, *, #3603, .F. ) ;
#16531 = VERTEX_POINT ( 'NONE', #15229 ) ;
#16532 = EDGE_CURVE ( 'NONE', #16605, #369, #1440, .T. ) ;
#16533 = ORIENTED_EDGE ( 'NONE', *, *, #8760, .F. ) ;
#16534 = DIRECTION ( 'NONE',  ( -0.7561779333270775005, -0.3559159372837353286, 0.5491072561318327550 ) ) ;
#16535 = CARTESIAN_POINT ( 'NONE',  ( 2.002547531651519996, -6.845637710436110801, -10.57595306287299763 ) ) ;
#16536 = AXIS2_PLACEMENT_3D ( 'NONE', #16791, #10881, #15261 ) ;
#16537 = CARTESIAN_POINT ( 'NONE',  ( 8.438534575730034959, -4.221456476902702981, 5.415535776177505589 ) ) ;
#16538 = CARTESIAN_POINT ( 'NONE',  ( 3.512766787570765548, -13.25664064834477429, 7.127386085302765295 ) ) ;
#16539 = DIRECTION ( 'NONE',  ( 0.000000000000000000, 0.000000000000000000, 1.000000000000000000 ) ) ;
#16540 = ORIENTED_EDGE ( 'NONE', *, *, #3580, .T. ) ;
#16541 = CARTESIAN_POINT ( 'NONE',  ( 0.3137051932979775248, 3.805684345189972895, -13.20008686438101719 ) ) ;
#16542 = EDGE_CURVE ( 'NONE', #10380, #9212, #5984, .T. ) ;
#16543 = CARTESIAN_POINT ( 'NONE',  ( 0.3058872367615226295, -7.578326039752520060, -11.46514199369366516 ) ) ;
#16544 = CARTESIAN_POINT ( 'NONE',  ( -2.864513242452084274, 7.499999999999999112, -15.84899838955092655 ) ) ;
#16545 = CARTESIAN_POINT ( 'NONE',  ( 16.57210152137263393, -0.01361613799508851197, -0.005118120558001528972 ) ) ;
#16546 = CARTESIAN_POINT ( 'NONE',  ( 1.254009781011571567, 1.011465182608068503, 14.64464726212582590 ) ) ;
#16547 = SURFACE_SIDE_STYLE ('',( #3628 ) ) ;
#16548 = CARTESIAN_POINT ( 'NONE',  ( 0.3150686449036065317, 13.01866258978842694, -4.391272911157185099 ) ) ;
#16549 = ORIENTED_EDGE ( 'NONE', *, *, #3270, .F. ) ;
#16551 = VERTEX_POINT ( 'NONE', #5182 ) ;
#16550 = CARTESIAN_POINT ( 'NONE',  ( -199.9999999999999716, 9.999999999999973355, 3.000000000000000000 ) ) ;
#16552 = CARTESIAN_POINT ( 'NONE',  ( 0.4862570985993235340, -3.580942890621579444, -13.44146924561384537 ) ) ;
#16553 = CARTESIAN_POINT ( 'NONE',  ( 0.3137051932979757485, -8.442169467526770887, -10.83767969834812561 ) ) ;
#16554 = CIRCLE ( 'NONE', #10439, 0.5000000000000004441 ) ;
#16555 = VERTEX_POINT ( 'NONE', #15405 ) ;
#16556 = DIRECTION ( 'NONE',  ( 0.5052478564545405115, 0.8629742774544859607, -0.000000000000000000 ) ) ;
#16557 = PRODUCT_DEFINITION_SHAPE ( 'NONE', 'NONE',  #18910 ) ;
#16558 = CARTESIAN_POINT ( 'NONE',  ( -4.482738663876439489, -5.389345431477982729, -11.99999999527192074 ) ) ;
#16559 = EDGE_CURVE ( 'NONE', #11365, #15356, #2349, .T. ) ;
#16560 = ORIENTED_EDGE ( 'NONE', *, *, #5425, .F. ) ;
#16561 = CARTESIAN_POINT ( 'NONE',  ( 16.56753206892534891, -0.006669401563384969034, 0.006760771273036147132 ) ) ;
#16562 = CARTESIAN_POINT ( 'NONE',  ( 0.3148213771069373057, 13.73693585713733967, 0.2297580318215192152 ) ) ;
#16563 = CARTESIAN_POINT ( 'NONE',  ( 2.636624412714237309, 11.10302021257826866, 11.60464335004050973 ) ) ;
#16564 = EDGE_CURVE ( 'NONE', #10137, #2339, #14169, .T. ) ;
#16565 = AXIS2_PLACEMENT_3D ( 'NONE', #15358, #8453, #15706 ) ;
#16566 = CARTESIAN_POINT ( 'NONE',  ( 1.847168016377980670, -9.955470380986684020, 7.464000291196382086 ) ) ;
#16567 = CARTESIAN_POINT ( 'NONE',  ( 15.00000000000000711, -39.99999999999999289, 0.000000000000000000 ) ) ;
#16569 = ORIENTED_EDGE ( 'NONE', *, *, #13199, .F. ) ;
#16568 = FACE_OUTER_BOUND ( 'NONE', #14653, .T. ) ;
#16570 = CARTESIAN_POINT ( 'NONE',  ( 0.3058872367615226295, 10.75034008168916166, 8.562166468153757037 ) ) ;
#16571 = VERTEX_POINT ( 'NONE', #15586 ) ;
#16572 = CARTESIAN_POINT ( 'NONE',  ( -199.9999999999999716, -30.00000000000003197, 0.000000000000000000 ) ) ;
#16573 = CARTESIAN_POINT ( 'NONE',  ( 0.8740764193766107359, 7.708542792189345683, 12.04241474977975557 ) ) ;
#16574 = ORIENTED_EDGE ( 'NONE', *, *, #15085, .F. ) ;
#16575 = ORIENTED_EDGE ( 'NONE', *, *, #2248, .F. ) ;
#16576 = FACE_OUTER_BOUND ( 'NONE', #1469, .T. ) ;
#16577 = ORIENTED_EDGE ( 'NONE', *, *, #9849, .T. ) ;
#16578 = LINE ( 'NONE', #526, #7486 ) ;
#16579 = ORIENTED_EDGE ( 'NONE', *, *, #14530, .T. ) ;
#16580 = CARTESIAN_POINT ( 'NONE',  ( 16.56872352241294521, -0.004564908236400289435, -0.009382111268606239951 ) ) ;
#16581 = EDGE_CURVE ( 'NONE', #9201, #2481, #18734, .T. ) ;
#16582 = B_SPLINE_CURVE_WITH_KNOTS ( 'NONE', 3,
 ( #4026, #9841, #15872, #15776, #12725, #1057, #5632, #2763, #17035, #8611, #5730, #1447, #11581 ),
 .UNSPECIFIED., .F., .F.,
 ( 4, 3, 3, 3, 4 ),
 ( 4.670885906470169154E-18, 0.0002299780670421044384, 0.0004599561239687884940, 0.0006896788984287876298, 0.0009194956271626387621 ),
 .UNSPECIFIED. ) ;
#16583 = CARTESIAN_POINT ( 'NONE',  ( 0.3145734862173260593, -13.73540602248380615, -0.3064017202076792512 ) ) ;
#16584 = DIRECTION ( 'NONE',  ( 0.000000000000000000, 0.000000000000000000, 1.000000000000000000 ) ) ;
#16585 = DIRECTION ( 'NONE',  ( -0.000000000000000000, -0.000000000000000000, 1.000000000000000000 ) ) ;
#16586 = VECTOR ( 'NONE', #17153, 1000.000000000000000 ) ;
#16587 = EDGE_CURVE ( 'NONE', #1103, #306, #9826, .T. ) ;
#16588 = CARTESIAN_POINT ( 'NONE',  ( 2.636624412715137922, -15.91454522070252153, 2.161493821597598508 ) ) ;
#16589 = CARTESIAN_POINT ( 'NONE',  ( 16.57778382496167424, -0.01482878558584693925, 0.001819584982831843212 ) ) ;
#16590 = CARTESIAN_POINT ( 'NONE',  ( 16.56753206892534891, -0.001549402974394229436, -0.009369540855502527313 ) ) ;
#16591 = CARTESIAN_POINT ( 'NONE',  ( 1.846138399168762101, -11.69739621335925328, 4.238866729160359448 ) ) ;
#16592 = CARTESIAN_POINT ( 'NONE',  ( 3.353306896162453477, -9.252610477110343012, 10.44017738170053278 ) ) ;
#16593 = FACE_OUTER_BOUND ( 'NONE', #8823, .T. ) ;
#16594 = CARTESIAN_POINT ( 'NONE',  ( 1.847372867223022963, -11.80112642014552371, -3.945260592619169948 ) ) ;
#16595 = ORIENTED_EDGE ( 'NONE', *, *, #12807, .T. ) ;
#16596 = ORIENTED_EDGE ( 'NONE', *, *, #5786, .F. ) ;
#16597 = EDGE_LOOP ( 'NONE', ( #5091, #57, #10990, #16635, #2995 ) ) ;
#16598 = VERTEX_POINT ( 'NONE', #18454 ) ;
#16599 = ORIENTED_EDGE ( 'NONE', *, *, #3458, .T. ) ;
#16600 = CARTESIAN_POINT ( 'NONE',  ( 1.959283090834841090, -7.909254450748933962, -9.750336807931228478 ) ) ;
#16601 = CARTESIAN_POINT ( 'NONE',  ( 0.3132642857406527370, 4.743831191224565202, -12.89240536501341161 ) ) ;
#16602 = ADVANCED_FACE ( 'NONE', ( #973 ), #2397, .F. ) ;
#16603 = CARTESIAN_POINT ( 'NONE',  ( 2.002547531651520885, 10.57595306287292480, 6.845637710436228929 ) ) ;
#16604 = EDGE_CURVE ( 'NONE', #16598, #12360, #1480, .T. ) ;
#16605 = VERTEX_POINT ( 'NONE', #16991 ) ;
#16606 = CARTESIAN_POINT ( 'NONE',  ( 1.959212340397940899, -3.239239832448945755, -12.12975361829679066 ) ) ;
#16607 = DIRECTION ( 'NONE',  ( 0.7561779333270775005, -0.3559159372837316093, -0.5491072561318351974 ) ) ;
#16608 = CARTESIAN_POINT ( 'NONE',  ( 1.977436885026095270, -6.153171729168663617, 14.12046670317548980 ) ) ;
#16609 = CARTESIAN_POINT ( 'NONE',  ( 2.697797270744666243, -11.26906156738832188, 7.053988368581824986 ) ) ;
#16610 = AXIS2_PLACEMENT_3D ( 'NONE', #2556, #14513, #1232 ) ;
#16611 = CARTESIAN_POINT ( 'NONE',  ( 16.56679352167444819, 0.001518074900130650254, -0.009170718284672547266 ) ) ;
#16612 = CARTESIAN_POINT ( 'NONE',  ( 2.949999999999999734, 0.000000000000000000, 0.000000000000000000 ) ) ;
#16613 = ORIENTED_EDGE ( 'NONE', *, *, #11594, .T. ) ;
#16614 = ORIENTED_EDGE ( 'NONE', *, *, #6035, .F. ) ;
#16615 = ORIENTED_EDGE ( 'NONE', *, *, #14312, .F. ) ;
#16616 = EDGE_LOOP ( 'NONE', ( #15902, #14372, #5700, #15870 ) ) ;
#16617 = DIRECTION ( 'NONE',  ( -1.000000000000000000, -0.000000000000000000, -0.000000000000000000 ) ) ;
#16618 = CARTESIAN_POINT ( 'NONE',  ( 16.56872352241294521, -0.001442253899401880124, -0.01033355228142401362 ) ) ;
#16619 = CIRCLE ( 'NONE', #7469, 2.499999999999995115 ) ;
#16620 = CARTESIAN_POINT ( 'NONE',  ( 2.636624412717140764, -2.862162146982851763, -15.80357026013259514 ) ) ;
#16621 = CARTESIAN_POINT ( 'NONE',  ( 2.002547531651519996, -6.845637710436110801, -10.57595306287299763 ) ) ;
#16622 = DIRECTION ( 'NONE',  ( 1.000000000000000000, 0.000000000000000000, 0.000000000000000000 ) ) ;
#16623 = ORIENTED_EDGE ( 'NONE', *, *, #12336, .T. ) ;
#16624 = ADVANCED_FACE ( 'NONE', ( #10266 ), #3743, .F. ) ;
#16625 = CARTESIAN_POINT ( 'NONE',  ( 1.254009781011254487, 14.64464726212552037, -1.011465182607978130 ) ) ;
#16626 = EDGE_CURVE ( 'NONE', #7234, #618, #8924, .T. ) ;
#16627 = CARTESIAN_POINT ( 'NONE',  ( 16.56782317627811096, 0.009228812961909594811, 0.003357783021327272015 ) ) ;
#16628 = EDGE_CURVE ( 'NONE', #14233, #16174, #13495, .T. ) ;
#16629 = CARTESIAN_POINT ( 'NONE',  ( -0.3286731010496698469, 6.995544057484794465, -12.00000000211882956 ) ) ;
#16630 = CARTESIAN_POINT ( 'NONE',  ( 16.56872352241294521, -0.009207754980063714498, -0.004907101719994726684 ) ) ;
#16631 = CARTESIAN_POINT ( 'NONE',  ( 0.3720661004400040439, 3.575426119359372823, -13.34435358167249142 ) ) ;
#16632 = CARTESIAN_POINT ( 'NONE',  ( 3.664313757352971379, -1.627055439596372777, 14.16986885736092461 ) ) ;
#16633 = CARTESIAN_POINT ( 'NONE',  ( 2.636624412716913390, 14.14563173255587536, -7.605649742760633991 ) ) ;
#16634 = VECTOR ( 'NONE', #6018, 1000.000000000000114 ) ;
#16635 = ORIENTED_EDGE ( 'NONE', *, *, #15446, .T. ) ;
#16636 = MANIFOLD_SOLID_BREP ( 'Hex', #17940 ) ;
#16638 = ORIENTED_EDGE ( 'NONE', *, *, #4472, .T. ) ;
#16637 = CARTESIAN_POINT ( 'NONE',  ( 16.56753206892534891, -0.004253784598196824578, -0.008490833999797990639 ) ) ;
#16639 = CARTESIAN_POINT ( 'NONE',  ( 0.3308579732647025096, 12.88563776947746398, 4.812490080619245880 ) ) ;
#16640 = VECTOR ( 'NONE', #10611, 1000.000000000000000 ) ;
#16641 = ORIENTED_EDGE ( 'NONE', *, *, #15873, .F. ) ;
#16642 = CARTESIAN_POINT ( 'NONE',  ( 0.8060261380167486056, -7.499999999999904077, -13.05296413415621615 ) ) ;
#16643 = ORIENTED_EDGE ( 'NONE', *, *, #3271, .T. ) ;
#16644 = CARTESIAN_POINT ( 'NONE',  ( 2.002547531651519996, -10.57595306287287329, -6.845637710436306200 ) ) ;
#16645 = CARTESIAN_POINT ( 'NONE',  ( 0.3142011359265305392, 13.73310835363014348, -0.3830873813806805472 ) ) ;
#16646 = AXIS2_PLACEMENT_3D ( 'NONE', #2773, #4325, #9954 ) ;
#16647 = CARTESIAN_POINT ( 'NONE',  ( -6.000000000000000000, 20.00000000000000000, 4.000000000000000000 ) ) ;
#16648 = CIRCLE ( 'NONE', #11759, 7.000000000000000000 ) ;
#16649 = CARTESIAN_POINT ( 'NONE',  ( 1.977436885025426694, 15.33079650480377154, 1.488549889121579817 ) ) ;
#16650 = AXIS2_PLACEMENT_3D ( 'NONE', #162, #8944, #10288 ) ;
#16651 = ADVANCED_FACE ( 'NONE', ( #14215 ), #6775, .F. ) ;
#16652 = PRESENTATION_STYLE_ASSIGNMENT (( #10732 ) ) ;
#16653 = CARTESIAN_POINT ( 'NONE',  ( 1.846613052777651198, -9.862487290071051405, 7.585914669018136713 ) ) ;
#16654 = B_SPLINE_CURVE_WITH_KNOTS ( 'NONE', 3,
 ( #3766, #18567, #5473, #8440, #14275, #8535 ),
 .UNSPECIFIED., .F., .F.,
 ( 4, 2, 4 ),
 ( 5.421010862427522170E-20, 0.0001828790815886950779, 0.0003657581631773901016 ),
 .UNSPECIFIED. ) ;
#16655 = CARTESIAN_POINT ( 'NONE',  ( 0.4862570985993235340, 0.7479633556564388996, -13.89016912371016765 ) ) ;
#16657 = VERTEX_POINT ( 'NONE', #238 ) ;
#16656 = CARTESIAN_POINT ( 'NONE',  ( 20.00000000000000711, -45.00000000000000000, 3.000000000000000000 ) ) ;
#16658 = DIRECTION ( 'NONE',  ( -0.000000000000000000, -1.000000000000000000, -0.000000000000000000 ) ) ;
#16659 = EDGE_LOOP ( 'NONE', ( #17473, #12318 ) ) ;
#16660 = CARTESIAN_POINT ( 'NONE',  ( 1.845755665166725068, 11.97169564665396280, -3.386720041070604204 ) ) ;
#16661 = CARTESIAN_POINT ( 'NONE',  ( 3.074695600507260984, -14.01296402267893448, 6.754521329824735076 ) ) ;
#16662 = AXIS2_PLACEMENT_3D ( 'NONE', #5334, #15465, #18066 ) ;
#16663 = ORIENTED_EDGE ( 'NONE', *, *, #8329, .T. ) ;
#16664 = VERTEX_POINT ( 'NONE', #1962 ) ;
#16665 = FACE_OUTER_BOUND ( 'NONE', #10901, .T. ) ;
#16666 = EDGE_CURVE ( 'NONE', #4207, #5898, #9680, .T. ) ;
#16667 = CARTESIAN_POINT ( 'NONE',  ( 2.353870697619111940, -6.980654702310762794, -10.90705766126227871 ) ) ;
#16668 = MANIFOLD_SOLID_BREP ( 'Cavity1', #4189 ) ;
#16669 = ORIENTED_EDGE ( 'NONE', *, *, #14386, .F. ) ;
#16670 = CARTESIAN_POINT ( 'NONE',  ( 3.950837973638677170, 1.958075594453790869, 14.41405733518061538 ) ) ;
#16671 = CARTESIAN_POINT ( 'NONE',  ( 3.950837973638677170, -1.958075594453692503, -14.41405733518062959 ) ) ;
#16672 = CARTESIAN_POINT ( 'NONE',  ( 0.000000000000000000, 0.000000000000000000, -12.00000000000000000 ) ) ;
#16673 = ADVANCED_FACE ( 'NONE', ( #1662 ), #18826, .T. ) ;
#16674 = CARTESIAN_POINT ( 'NONE',  ( 8.522092701127531811, 5.841710761610131364, 3.777034505568545253 ) ) ;
#16675 = CARTESIAN_POINT ( 'NONE',  ( 3.950837973638668288, 0.000000000000000000, 0.000000000000000000 ) ) ;
#16676 = ADVANCED_FACE ( 'NONE', ( #6259 ), #12137, .T. ) ;
#16677 = ADVANCED_FACE ( 'NONE', ( #11896 ), #8376, .F. ) ;
#16678 = VECTOR ( 'NONE', #10170, 1000.000000000000000 ) ;
#16679 = CARTESIAN_POINT ( 'NONE',  ( -1.500000000000000000, -2.869946927167511679E-16, 5.000000000000000000 ) ) ;
#16680 = APPLICATION_PROTOCOL_DEFINITION ( 'draft international standard', 'automotive_design', 1998, #18754 ) ;
#16681 = PRESENTATION_LAYER_ASSIGNMENT (  '', '', ( #9351 ) ) ;
#16682 =( NAMED_UNIT ( * ) PLANE_ANGLE_UNIT ( ) SI_UNIT ( $, .RADIAN. ) );
#16683 = CARTESIAN_POINT ( 'NONE',  ( 0.3720661004400040439, 7.524064345033631973, -11.58636699658207370 ) ) ;
#16684 = CARTESIAN_POINT ( 'NONE',  ( 3.074695600507584281, 13.70113613813179043, -7.366518011945612621 ) ) ;
#16685 = CARTESIAN_POINT ( 'NONE',  ( 0.4754618798421162973, -8.775436892861034011, -10.80499583390522567 ) ) ;
#16686 = CARTESIAN_POINT ( 'NONE',  ( 0.3132635586635975078, 8.495712071659401232, 10.79541209008106861 ) ) ;
#16687 = CARTESIAN_POINT ( 'NONE',  ( 0.3137051932979792457, -13.20008686438103140, -3.805684345189927154 ) ) ;
#16688 = VERTEX_POINT ( 'NONE', #11800 ) ;
#16689 = EDGE_CURVE ( 'NONE', #5119, #7915, #15475, .T. ) ;
#16690 = EDGE_LOOP ( 'NONE', ( #15124, #6776 ) ) ;
#16691 = ORIENTED_EDGE ( 'NONE', *, *, #567, .T. ) ;
#16692 = VERTEX_POINT ( 'NONE', #9313 ) ;
#16693 = VERTEX_POINT ( 'NONE', #532 ) ;
#16694 = ADVANCED_FACE ( 'NONE', ( #4921 ), #10661, .T. ) ;
#16695 = DIRECTION ( 'NONE',  ( 0.000000000000000000, 0.000000000000000000, -1.000000000000000000 ) ) ;
#16696 = CARTESIAN_POINT ( 'NONE',  ( -6.231098469233190329, -7.499999999999999112, -16.99999999999999645 ) ) ;
#16697 = AXIS2_PLACEMENT_3D ( 'NONE', #15307, #15224, #8062 ) ;
#16698 = CARTESIAN_POINT ( 'NONE',  ( -20.00000000000000000, 2.499999999999998668, -17.00000000000000000 ) ) ;
#16699 = DIRECTION ( 'NONE',  ( 0.7561779333270775005, -0.6106991889125055195, -0.2350349629540206264 ) ) ;
#16700 = VECTOR ( 'NONE', #12305, 1000.000000000000000 ) ;
#16701 = AXIS2_PLACEMENT_3D ( 'NONE', #9089, #496, #3541 ) ;
#16702 = CARTESIAN_POINT ( 'NONE',  ( 3.950837973638676281, -12.81214529934970336, -6.888253895133431115 ) ) ;
#16703 = DIRECTION ( 'NONE',  ( -1.000000000000000000, -0.000000000000000000, -0.000000000000000000 ) ) ;
#16704 = CARTESIAN_POINT ( 'NONE',  ( -5.000000000000000000, 0.000000000000000000, 0.000000000000000000 ) ) ;
#16705 = CARTESIAN_POINT ( 'NONE',  ( 2.002547531651519996, 10.57595306287302250, -6.845637710436074386 ) ) ;
#16706 = VECTOR ( 'NONE', #18265, 1000.000000000000000 ) ;
#16707 = ORIENTED_EDGE ( 'NONE', *, *, #9112, .F. ) ;
#16709 = B_SPLINE_CURVE_WITH_KNOTS ( 'NONE', 3,
 ( #6960, #5233, #2363, #3983, #11168, #16804 ),
 .UNSPECIFIED., .F., .F.,
 ( 4, 2, 4 ),
 ( 8.673617379884035472E-19, 0.001500839035891551572, 0.003001678071783102277 ),
 .UNSPECIFIED. ) ;
#16708 = PRODUCT_DEFINITION_SHAPE ( 'NONE', 'NONE',  #18906 ) ;
#16710 = B_SPLINE_CURVE_WITH_KNOTS ( 'NONE', 3,
 ( #7715, #6459, #13522, #1875, #16500, #9421 ),
 .UNSPECIFIED., .F., .F.,
 ( 4, 2, 4 ),
 ( 0.000000000000000000, 0.001500839035891550922, 0.003001678071783101844 ),
 .UNSPECIFIED. ) ;
#16711 = VERTEX_POINT ( 'NONE', #2058 ) ;
#16712 = EDGE_CURVE ( 'NONE', #6853, #11007, #12814, .T. ) ;
#16713 = ORIENTED_EDGE ( 'NONE', *, *, #18030, .T. ) ;
#16714 = AXIS2_PLACEMENT_3D ( 'NONE', #12928, #1270, #2693 ) ;
#16715 = EDGE_LOOP ( 'NONE', ( #9895, #3172, #1328, #8374 ) ) ;
#16716 = DIRECTION ( 'NONE',  ( 1.000000000000000000, 0.000000000000000000, 0.000000000000000000 ) ) ;
#16717 = AXIS2_PLACEMENT_3D ( 'NONE', #16282, #2872, #14551 ) ;
#16718 = CARTESIAN_POINT ( 'NONE',  ( 0.4754618798421167414, 11.68486377711977298, -7.564402563418342496 ) ) ;
#16719 = CARTESIAN_POINT ( 'NONE',  ( 0.3137051932979809665, -13.20008686438108647, 3.805684345189735307 ) ) ;
#16720 = LINE ( 'NONE', #3620, #9143 ) ;
#16721 = CARTESIAN_POINT ( 'NONE',  ( 0.000000000000000000, 0.000000000000000000, 7.000000000000000000 ) ) ;
#16722 = ORIENTED_EDGE ( 'NONE', *, *, #8065, .T. ) ;
#16723 = CARTESIAN_POINT ( 'NONE',  ( 16.56872352241294521, -0.001821578298043862289, 0.01027347319884366027 ) ) ;
#16724 = CARTESIAN_POINT ( 'NONE',  ( 0.3308579732647018989, 11.46737410776364996, -7.595989242675004860 ) ) ;
#16725 = CARTESIAN_POINT ( 'NONE',  ( -5.783659440658965423, 3.949482697158818389, -11.99999999872357748 ) ) ;
#16726 = FACE_OUTER_BOUND ( 'NONE', #18348, .T. ) ;
#16727 = CONICAL_SURFACE ( 'NONE', #854, 2.500000000000000000, 1.029744258676656754 ) ;
#16728 = CARTESIAN_POINT ( 'NONE',  ( 16.56753206892534891, -0.006760771273035160941, 0.006669401563385170262 ) ) ;
#16729 = FILL_AREA_STYLE ('',( #17978 ) ) ;
#16730 = CARTESIAN_POINT ( 'NONE',  ( 2.636624412715435462, -15.80357026013316712, -2.862162146983298516 ) ) ;
#16731 = ORIENTED_EDGE ( 'NONE', *, *, #10831, .T. ) ;
#16733 = ORIENTED_EDGE ( 'NONE', *, *, #16473, .F. ) ;
#16732 = CARTESIAN_POINT ( 'NONE',  ( 1.847412631396507798, 11.84727953344288132, -3.804043368582538776 ) ) ;
#16734 = CARTESIAN_POINT ( 'NONE',  ( 8.438534575730034959, 6.454982381540319558, -2.341351102130211359 ) ) ;
#16735 = EDGE_CURVE ( 'NONE', #978, #819, #7990, .T. ) ;
#16736 = ADVANCED_FACE ( 'NONE', ( #13795 ), #10446, .F. ) ;
#16737 = AXIS2_PLACEMENT_3D ( 'NONE', #1644, #8720, #7489 ) ;
#16738 = ORIENTED_EDGE ( 'NONE', *, *, #9427, .F. ) ;
#16739 = DIRECTION ( 'NONE',  ( 0.000000000000000000, 0.000000000000000000, 1.000000000000000000 ) ) ;
#16740 = CARTESIAN_POINT ( 'NONE',  ( -3.601232060343992014, -7.499999999999612754, -13.21583132166217744 ) ) ;
#16741 = ORIENTED_EDGE ( 'NONE', *, *, #2294, .F. ) ;
#16742 = CARTESIAN_POINT ( 'NONE',  ( 0.4862570985993252548, -12.97920246947875889, -5.003653737315625349 ) ) ;
#16743 = CARTESIAN_POINT ( 'NONE',  ( 0.8740779401510443414, -12.04241618260075164, -7.708543377337893077 ) ) ;
#16744 = CARTESIAN_POINT ( 'NONE',  ( 2.002547531651519996, -4.532360870844247991, -11.75462648437106417 ) ) ;
#16745 = PLANE ( 'NONE',  #11454 ) ;
#16746 = AXIS2_PLACEMENT_3D ( 'NONE', #4627, #14943, #3565 ) ;
#16747 = SURFACE_STYLE_FILL_AREA ( #3358 ) ;
#16748 = FACE_OUTER_BOUND ( 'NONE', #16334, .T. ) ;
#16750 = ORIENTED_EDGE ( 'NONE', *, *, #130, .T. ) ;
#16749 = CARTESIAN_POINT ( 'NONE',  ( 0.3132642857406489623, -11.41580579227782444, 7.641821025099830855 ) ) ;
#16751 = DIRECTION ( 'NONE',  ( 0.000000000000000000, 0.000000000000000000, 1.000000000000000000 ) ) ;
#16752 = ORIENTED_EDGE ( 'NONE', *, *, #14977, .F. ) ;
#16753 = DIRECTION ( 'NONE',  ( -1.000000000000000000, 0.000000000000000000, 0.000000000000000000 ) ) ;
#16754 = CARTESIAN_POINT ( 'NONE',  ( 1.918918678667048683, -11.69059232068581800, 4.466049546133867842 ) ) ;
#16755 = ORIENTED_EDGE ( 'NONE', *, *, #8086, .T. ) ;
#16756 = ORIENTED_EDGE ( 'NONE', *, *, #12638, .F. ) ;
#16757 = DIRECTION ( 'NONE',  ( -0.000000000000000000, -0.000000000000000000, 1.000000000000000000 ) ) ;
#16758 = ADVANCED_FACE ( 'NONE', ( #13886 ), #5191, .T. ) ;
#16759 = DIRECTION ( 'NONE',  ( -1.000000000000000000, -0.000000000000000000, -0.000000000000000000 ) ) ;
#16760 = MANIFOLD_SOLID_BREP ( 'Hex', #16412 ) ;
#16761 = ADVANCED_BREP_SHAPE_REPRESENTATION ( '', ( #16154, #2030 ), #5382 ) ;
#16762 = ORIENTED_EDGE ( 'NONE', *, *, #7372, .F. ) ;
#16763 = CARTESIAN_POINT ( 'NONE',  ( 3.950837973638668288, 14.41405733518061716, 1.958075594453843493 ) ) ;
#16764 = CARTESIAN_POINT ( 'NONE',  ( 1.342453679581834924, -12.51077660954460136, -7.902645620902585932 ) ) ;
#16765 = CIRCLE ( 'NONE', #7664, 5.000000000000000000 ) ;
#16766 = DIRECTION ( 'NONE',  ( 0.000000000000000000, 0.000000000000000000, 1.000000000000000000 ) ) ;
#16767 = CARTESIAN_POINT ( 'NONE',  ( 1.560000000000000053, -0.8660254037844384856, -1.500000000000000000 ) ) ;
#16768 = ADVANCED_FACE ( 'NONE', ( #12274, #803 ), #711, .F. ) ;
#16769 = CARTESIAN_POINT ( 'NONE',  ( 1.847412631396501803, 7.278870946904251404, 10.09191835241965407 ) ) ;
#16770 = APPLICATION_PROTOCOL_DEFINITION ( 'draft international standard', 'automotive_design', 1998, #5094 ) ;
#16771 = CARTESIAN_POINT ( 'NONE',  ( 2.353870697619112384, 12.92712089195302738, 0.7635393531606785578 ) ) ;
#16772 = CARTESIAN_POINT ( 'NONE',  ( -55.93192566395838128, 4.999999999999974243, 6.000000000000000000 ) ) ;
#16773 = CARTESIAN_POINT ( 'NONE',  ( 0.3058872367615230181, -12.87003593440631732, 4.821066432589277362 ) ) ;
#16774 = CARTESIAN_POINT ( 'NONE',  ( 8.522092701127531811, -6.489356537178209372, 2.505958102592595882 ) ) ;
#16775 = B_SPLINE_CURVE_WITH_KNOTS ( 'NONE', 3,
 ( #1624, #104, #1827, #17700, #3040, #6130, #11667, #4506, #11765, #14912 ),
 .UNSPECIFIED., .F., .F.,
 ( 4, 3, 3, 4 ),
 ( 0.0004597478348664300451, 0.0004599561239687907166, 0.0006896788984287883888, 0.0009194956271626400631 ),
 .UNSPECIFIED. ) ;
#16776 = CARTESIAN_POINT ( 'NONE',  ( 20.00000000000000711, -45.00000000000000000, 0.000000000000000000 ) ) ;
#16777 = VECTOR ( 'NONE', #12300, 1000.000000000000000 ) ;
#16778 = ADVANCED_FACE ( 'NONE', ( #5100 ), #14967, .F. ) ;
#16779 = EDGE_LOOP ( 'NONE', ( #11841, #18828, #4226, #7777 ) ) ;
#16780 = ORIENTED_EDGE ( 'NONE', *, *, #18168, .T. ) ;
#16781 = EDGE_CURVE ( 'NONE', #3169, #998, #11227, .T. ) ;
#16782 = EDGE_CURVE ( 'NONE', #15522, #6394, #1174, .T. ) ;
#16783 = ORIENTED_EDGE ( 'NONE', *, *, #11830, .F. ) ;
#16784 =( BOUNDED_SURFACE ( )  B_SPLINE_SURFACE ( 3, 1, ( 
 ( #2715, #11340 ),
 ( #8468, #15913 ),
 ( #12763, #18586 ),
 ( #14299, #4067 ) ),
 .UNSPECIFIED., .F., .F., .T. ) 
 B_SPLINE_SURFACE_WITH_KNOTS ( ( 4, 4 ),
 ( 2, 2 ),
 ( 0.000000000000000000, 1.000000000000000000 ),
 ( 0.000000000000000000, 1.000000000000000000 ),
 .UNSPECIFIED. ) 
 GEOMETRIC_REPRESENTATION_ITEM ( )  RATIONAL_B_SPLINE_SURFACE ( (
 ( 1.000000000000000000, 1.000000000000000000),
 ( 0.7792777138730158093, 0.9689936506012928330),
 ( 0.7792777138730158093, 0.9689936506012928330),
 ( 1.000000000000000000, 1.000000000000000000) ) ) 
 REPRESENTATION_ITEM ( '' )  SURFACE ( )  );
#16785 = ORIENTED_EDGE ( 'NONE', *, *, #1777, .F. ) ;
#16786 = B_SPLINE_CURVE_WITH_KNOTS ( 'NONE', 3,
 ( #4832, #16493, #8741, #336, #6069, #7707, #17734, #4438, #4638, #10366, #140, #14659, #10268 ),
 .UNSPECIFIED., .F., .F.,
 ( 4, 3, 3, 3, 4 ),
 ( 2.602085213965210642E-18, 0.0002299780670421064713, 0.0004599561239687913672, 0.0006896788984287877382, 0.0009194956271626401716 ),
 .UNSPECIFIED. ) ;
#16787 = CARTESIAN_POINT ( 'NONE',  ( 1.846613052777650976, -0.3401093050880946711, -12.43780859207240219 ) ) ;
#16788 = CARTESIAN_POINT ( 'NONE',  ( 0.6293707761309761395, -7.500000000000001776, -14.32724244806440517 ) ) ;
#16789 = ORIENTED_EDGE ( 'NONE', *, *, #4153, .F. ) ;
#16790 = CARTESIAN_POINT ( 'NONE',  ( 0.8740764193768816304, 0.8420116711623857331, -14.27348595579795010 ) ) ;
#16791 = CARTESIAN_POINT ( 'NONE',  ( 0.000000000000000000, 0.000000000000000000, 10.49999999999999822 ) ) ;
#16792 = EDGE_CURVE ( 'NONE', #10630, #12492, #5494, .T. ) ;
#16793 = CARTESIAN_POINT ( 'NONE',  ( 20.00000000000000000, -2.500000000000000444, -22.00000000000000000 ) ) ;
#16794 = DIRECTION ( 'NONE',  ( 1.000000000000000000, 0.000000000000000000, 0.000000000000000000 ) ) ;
#16795 = CARTESIAN_POINT ( 'NONE',  ( 1.845755665166724624, -7.694641135842892332, 9.776700214453605042 ) ) ;
#16796 = CARTESIAN_POINT ( 'NONE',  ( 22.30499999999999972, 3.061616997868384620E-16, -2.500000000000001332 ) ) ;
#16797 = CARTESIAN_POINT ( 'NONE',  ( 3.686287386450715076E-15, -27.00000000000000000, 21.01316734529526187 ) ) ;
#16798 = ORIENTED_EDGE ( 'NONE', *, *, #10049, .T. ) ;
#16799 = ORIENTED_EDGE ( 'NONE', *, *, #1071, .T. ) ;
#16800 = ORIENTED_EDGE ( 'NONE', *, *, #5194, .F. ) ;
#16801 = ORIENTED_EDGE ( 'NONE', *, *, #1832, .F. ) ;
#16802 = CARTESIAN_POINT ( 'NONE',  ( 2.636624412716062071, -11.10302021258080352, -11.60464335004061454 ) ) ;
#16803 = CIRCLE ( 'NONE', #6745, 2.499999999999999556 ) ;
#16804 = CARTESIAN_POINT ( 'NONE',  ( 3.950837973638675393, -13.10350451991835818, -6.316429227969608817 ) ) ;
#16805 = CARTESIAN_POINT ( 'NONE',  ( 0.3095370825347224519, -13.73357284481725138, 0.4597470195089713441 ) ) ;
#16806 = CARTESIAN_POINT ( 'NONE',  ( 1.846138399168762101, 11.95493567637855392, -3.446241763652874379 ) ) ;
#16807 = ORIENTED_EDGE ( 'NONE', *, *, #18523, .T. ) ;
#16808 = CARTESIAN_POINT ( 'NONE',  ( 16.57210152137263393, 0.01136813053532160708, -0.009075239946109073599 ) ) ;
#16809 = EDGE_CURVE ( 'NONE', #9356, #11185, #15686, .T. ) ;
#16810 = CARTESIAN_POINT ( 'NONE',  ( 0.4385251269669942498, 11.63205320541534071, -7.540955776459614235 ) ) ;
#16811 = CARTESIAN_POINT ( 'NONE',  ( 0.03525595549292682984, 7.499999999999999112, -14.17755750872172271 ) ) ;
#16812 = CARTESIAN_POINT ( 'NONE',  ( 1.977436885026782276, -7.806953934146112495, -13.27782258181927233 ) ) ;
#16813 = CARTESIAN_POINT ( 'NONE',  ( 1.846138399168762101, -9.815003036200353748, -7.646096044340000120 ) ) ;
#16814 = EDGE_CURVE ( 'NONE', #2805, #14769, #9850, .T. ) ;
#16815 = DIRECTION ( 'NONE',  ( 1.000000000000000000, 0.000000000000000000, -0.000000000000000000 ) ) ;
#16816 = SHAPE_REPRESENTATION ( 'Soft-Grip Handle Sleeve Overmolds (x2)', ( #2030 ), #5983 ) ;
#16817 = CARTESIAN_POINT ( 'NONE',  ( 1.861628059977343153, -4.358833901513129661, 11.66985327793197236 ) ) ;
#16818 = ORIENTED_EDGE ( 'NONE', *, *, #17001, .T. ) ;
#16819 = APPLICATION_CONTEXT ( 'automotive_design' ) ;
#16821 = ORIENTED_EDGE ( 'NONE', *, *, #16964, .T. ) ;
#16820 = CARTESIAN_POINT ( 'NONE',  ( 0.8740779401510754276, -9.070947476926809472, -11.05257166392059354 ) ) ;
#16822 = CARTESIAN_POINT ( 'NONE',  ( 2.636624412715137034, -11.60464335004055947, 11.10302021257951743 ) ) ;
#16823 = CARTESIAN_POINT ( 'NONE',  ( 1.847372867223026294, -0.1054171785007356615, 12.44269075185938789 ) ) ;
#16824 = ORIENTED_EDGE ( 'NONE', *, *, #8028, .F. ) ;
#16825 = LINE ( 'NONE', #8588, #1824 ) ;
#16826 = CARTESIAN_POINT ( 'NONE',  ( -2.564349062531098067, -7.500000000000000888, -15.65236830614252028 ) ) ;
#16827 = ORIENTED_EDGE ( 'NONE', *, *, #5395, .T. ) ;
#16828 = CARTESIAN_POINT ( 'NONE',  ( 2.320520222539028232, 15.43440824797023225, -3.126729907237324912 ) ) ;
#16829 = CARTESIAN_POINT ( 'NONE',  ( 2.320521194583335500, -13.71278319228129483, -7.743190876766059105 ) ) ;
#16830 = DIRECTION ( 'NONE',  ( 0.000000000000000000, -1.000000000000000000, 0.000000000000000000 ) ) ;
#16831 = CARTESIAN_POINT ( 'NONE',  ( 1.846613052777650976, 9.862487290071108248, -7.585914669018062106 ) ) ;
#16832 = EDGE_CURVE ( 'NONE', #17922, #15093, #16917, .T. ) ;
#16833 = EDGE_CURVE ( 'NONE', #11886, #1087, #16803, .T. ) ;
#16834 = EDGE_CURVE ( 'NONE', #5002, #3017, #18560, .T. ) ;
#16835 = AXIS2_PLACEMENT_3D ( 'NONE', #7781, #6346, #15027 ) ;
#16836 = PRESENTATION_STYLE_ASSIGNMENT (( #11109 ) ) ;
#16837 = CARTESIAN_POINT ( 'NONE',  ( 16.58200780006414732, -0.002844973367391502410, 0.01080144354108869553 ) ) ;
#16838 = CARTESIAN_POINT ( 'NONE',  ( 0.3095370825347224519, 7.700448427572037069, -11.38092634279620263 ) ) ;
#16840 = ORIENTED_EDGE ( 'NONE', *, *, #9691, .F. ) ;
#16839 = FACE_OUTER_BOUND ( 'NONE', #17686, .T. ) ;
#16841 = CARTESIAN_POINT ( 'NONE',  ( 1.254009781012375813, 11.25324419414251942, -9.426200207652035701 ) ) ;
#16842 = CARTESIAN_POINT ( 'NONE',  ( 0.3170788640506441158, 4.100430649998145327, -13.11595226728153385 ) ) ;
#16843 = CARTESIAN_POINT ( 'NONE',  ( 1.918921323896323194, 12.08297777410669482, -3.258415356426395793 ) ) ;
#16844 = LINE ( 'NONE', #12353, #17012 ) ;
#16845 = ORIENTED_EDGE ( 'NONE', *, *, #10379, .T. ) ;
#16846 = ORIENTED_EDGE ( 'NONE', *, *, #4670, .F. ) ;
#16847 = CARTESIAN_POINT ( 'NONE',  ( 2.636624412714994037, -14.46769361191274328, -6.973567714907344950 ) ) ;
#16848 = EDGE_LOOP ( 'NONE', ( #16663, #10333 ) ) ;
#16849 = CARTESIAN_POINT ( 'NONE',  ( 2.123976203522053741, -1.531817366691644144, -15.54801196254788742 ) ) ;
#16850 = CARTESIAN_POINT ( 'NONE',  ( 0.3095370825347233956, -13.73357284481725138, 0.4597470195089733425 ) ) ;
#16851 = DIRECTION ( 'NONE',  ( -0.000000000000000000, -1.000000000000000000, -0.000000000000000000 ) ) ;
#16852 = AXIS2_PLACEMENT_3D ( 'NONE', #8403, #2461, #9738 ) ;
#16853 = DIRECTION ( 'NONE',  ( -0.000000000000000000, -1.000000000000000000, -0.000000000000000000 ) ) ;
#16854 = EDGE_CURVE ( 'NONE', #17922, #13924, #11311, .T. ) ;
#16855 = CARTESIAN_POINT ( 'NONE',  ( 16.58200780006414732, 0.002844973367391573534, -0.01080144354108867819 ) ) ;
#16856 = CARTESIAN_POINT ( 'NONE',  ( 1.847168016377982003, 7.464000291196414061, 9.955470380986653822 ) ) ;
#16857 = EDGE_CURVE ( 'NONE', #7506, #8066, #15836, .T. ) ;
#16858 = B_SPLINE_CURVE_WITH_KNOTS ( 'NONE', 3,
 ( #16322, #7922, #9342, #13734, #644, #15168 ),
 .UNSPECIFIED., .F., .F.,
 ( 4, 2, 4 ),
 ( 3.671973638477265170E-17, 0.0001825746017570593200, 0.0003651492035140796086 ),
 .UNSPECIFIED. ) ;
#16859 =( NAMED_UNIT ( * ) SI_UNIT ( $, .STERADIAN. ) SOLID_ANGLE_UNIT ( ) );
#16860 = DIRECTION ( 'NONE',  ( 0.000000000000000000, 0.000000000000000000, 1.000000000000000000 ) ) ;
#16861 = DIRECTION ( 'NONE',  ( 0.000000000000000000, 0.000000000000000000, 1.000000000000000000 ) ) ;
#16862 = EDGE_CURVE ( 'NONE', #5180, #4027, #8431, .T. ) ;
#16863 = CARTESIAN_POINT ( 'NONE',  ( 1.846613052777651198, 7.035606253495462425, -10.26230975746752350 ) ) ;
#16864 = CARTESIAN_POINT ( 'NONE',  ( 2.002547531651520885, -4.532360870844412304, 11.75462648437100377 ) ) ;
#16865 = CARTESIAN_POINT ( 'NONE',  ( 2.353870697619111496, -10.90705766126224674, 6.980654702310806314 ) ) ;
#16866 = CARTESIAN_POINT ( 'NONE',  ( 1.846138399168762101, -10.30487220521574976, 6.971848976710974810 ) ) ;
#16867 = EDGE_CURVE ( 'NONE', #4709, #7061, #14269, .T. ) ;
#16868 = ORIENTED_EDGE ( 'NONE', *, *, #4644, .F. ) ;
#16869 = ORIENTED_EDGE ( 'NONE', *, *, #9182, .T. ) ;
#16870 = ORIENTED_EDGE ( 'NONE', *, *, #2425, .F. ) ;
#16871 = B_SPLINE_CURVE_WITH_KNOTS ( 'NONE', 3,
 ( #13592, #10642, #5080, #511, #18089, #14929 ),
 .UNSPECIFIED., .F., .F.,
 ( 4, 2, 4 ),
 ( 0.000000000000000000, 0.0001828790815886942919, 0.0003657581631773885837 ),
 .UNSPECIFIED. ) ;
#16872 = ORIENTED_EDGE ( 'NONE', *, *, #7912, .T. ) ;
#16873 = COLOUR_RGB ( '', 0.08235294, 0.09019608, 0.10196078) ;
#16874 = CARTESIAN_POINT ( 'NONE',  ( 0.3137051932979809665, 10.83767969834803324, 8.442169467526891680 ) ) ;
#16875 = CARTESIAN_POINT ( 'NONE',  ( 0.1940040276537112751, -7.500000000000000000, -14.18536928022392019 ) ) ;
#16876 = CARTESIAN_POINT ( 'NONE',  ( 25.00000000000000000, -7.500000000000000888, -16.99999999999999645 ) ) ;
#16877 = CARTESIAN_POINT ( 'NONE',  ( 2.750000000000000000, 2.499999999999999112, 0.000000000000000000 ) ) ;
#16878 = CARTESIAN_POINT ( 'NONE',  ( 3.950837973638676281, 12.81214529934975310, 6.888253895133341409 ) ) ;
#16879 = DIRECTION ( 'NONE',  ( 0.7635533937278214944, -0.5095610256143857653, -0.3966532189476615899 ) ) ;
#16880 = EDGE_CURVE ( 'NONE', #1187, #9395, #16765, .T. ) ;
#16881 = ORIENTED_EDGE ( 'NONE', *, *, #3438, .T. ) ;
#16882 = CARTESIAN_POINT ( 'NONE',  ( 0.4862570985993235340, 8.769551628660890330, -10.79774104611363761 ) ) ;
#16883 = CARTESIAN_POINT ( 'NONE',  ( 2.636624412715137922, -6.973567714907947135, 14.46769361191283920 ) ) ;
#16884 = VECTOR ( 'NONE', #14357, 1000.000000000000000 ) ;
#16885 = VERTEX_POINT ( 'NONE', #2962 ) ;
#16886 =( BOUNDED_SURFACE ( )  B_SPLINE_SURFACE ( 3, 1, ( 
 ( #11484, #3043 ),
 ( #5631, #106 ),
 ( #5923, #14435 ),
 ( #8890, #15871 ) ),
 .UNSPECIFIED., .F., .F., .T. ) 
 B_SPLINE_SURFACE_WITH_KNOTS ( ( 4, 4 ),
 ( 2, 2 ),
 ( 0.000000000000000000, 1.000000000000000000 ),
 ( 0.000000000000000000, 1.000000000000000000 ),
 .UNSPECIFIED. ) 
 GEOMETRIC_REPRESENTATION_ITEM ( )  RATIONAL_B_SPLINE_SURFACE ( (
 ( 1.000000000000000000, 1.000000000000000000),
 ( 0.9593108457356467333, 0.9995965569486454649),
 ( 0.9593108457356467333, 0.9995965569486454649),
 ( 1.000000000000000000, 1.000000000000000000) ) ) 
 REPRESENTATION_ITEM ( '' )  SURFACE ( )  );
#16887 = ORIENTED_EDGE ( 'NONE', *, *, #18523, .F. ) ;
#16888 = ORIENTED_EDGE ( 'NONE', *, *, #13222, .T. ) ;
#16889 = ORIENTED_EDGE ( 'NONE', *, *, #2756, .F. ) ;
#16890 = DIRECTION ( 'NONE',  ( -0.000000000000000000, -0.000000000000000000, -1.000000000000000000 ) ) ;
#16891 = EDGE_CURVE ( 'NONE', #10630, #16551, #13009, .T. ) ;
#16892 = FACE_OUTER_BOUND ( 'NONE', #10203, .T. ) ;
#16893 = CARTESIAN_POINT ( 'NONE',  ( 1.846138399168762101, 9.815003036200520725, -7.646096044339786069 ) ) ;
#16894 = CARTESIAN_POINT ( 'NONE',  ( 20.00000000000000000, 2.499999999999998668, -16.99999999999999645 ) ) ;
#16895 = FILL_AREA_STYLE ('',( #12584 ) ) ;
#16896 = ORIENTED_EDGE ( 'NONE', *, *, #9707, .T. ) ;
#16897 = CARTESIAN_POINT ( 'NONE',  ( 1.562796894703937678, 0.000000000000000000, -12.15840553252917289 ) ) ;
#16898 = AXIS2_PLACEMENT_3D ( 'NONE', #11856, #2, #6028 ) ;
#16899 = DIRECTION ( 'NONE',  ( -1.000000000000000000, -0.000000000000000000, -6.938893903907227392E-16 ) ) ;
#16900 = CARTESIAN_POINT ( 'NONE',  ( -0.6634400264848326900, 7.499999999999671374, -13.04619536630290533 ) ) ;
#16901 = CARTESIAN_POINT ( 'NONE',  ( 16.57210152137263393, 0.01453130299868522594, 0.0006600038696346533949 ) ) ;
#16902 = B_SPLINE_CURVE_WITH_KNOTS ( 'NONE', 3,
 ( #2044, #15034, #1951, #13602, #3562, #12082 ),
 .UNSPECIFIED., .F., .F.,
 ( 4, 2, 4 ),
 ( 0.000000000000000000, 0.001500839035891551139, 0.003001678071783102277 ),
 .UNSPECIFIED. ) ;
#16903 = FACE_OUTER_BOUND ( 'NONE', #4725, .T. ) ;
#16904 = DIRECTION ( 'NONE',  ( -0.000000000000000000, -0.000000000000000000, -1.000000000000000000 ) ) ;
#16905 = CARTESIAN_POINT ( 'NONE',  ( 0.3150692679895968906, 13.11337225490258263, -4.099798979280710576 ) ) ;
#16906 = CARTESIAN_POINT ( 'NONE',  ( 19.99999999999999645, 15.00000000000000000, 0.000000000000000000 ) ) ;
#16907 = ORIENTED_EDGE ( 'NONE', *, *, #4135, .F. ) ;
#16909 = VERTEX_POINT ( 'NONE', #17219 ) ;
#16908 = DIRECTION ( 'NONE',  ( 0.000000000000000000, 0.000000000000000000, 1.000000000000000000 ) ) ;
#16910 = CARTESIAN_POINT ( 'NONE',  ( 16.56753206892534891, -0.001421777558676855365, -0.009389754735541546229 ) ) ;
#16911 = EDGE_CURVE ( 'NONE', #12492, #4457, #2545, .T. ) ;
#16912 = AXIS2_PLACEMENT_3D ( 'NONE', #1304, #5690, #18692 ) ;
#16913 = DIRECTION ( 'NONE',  ( 0.000000000000000000, 0.000000000000000000, 1.000000000000000000 ) ) ;
#16914 = ORIENTED_EDGE ( 'NONE', *, *, #10426, .F. ) ;
#16915 = DIRECTION ( 'NONE',  ( 0.7561779333270775005, 0.6106991889125038542, 0.2350349629540249285 ) ) ;
#16916 = CARTESIAN_POINT ( 'NONE',  ( -4.449459268825699532, -7.500000000000000888, -16.63368482084344890 ) ) ;
#16917 = B_SPLINE_CURVE_WITH_KNOTS ( 'NONE', 3,
 ( #8527, #13111, #1168, #18647, #4324, #14445 ),
 .UNSPECIFIED., .F., .F.,
 ( 4, 2, 4 ),
 ( 4.063025038712889623E-17, 0.0002014099069817291640, 0.0004028198139634176704 ),
 .UNSPECIFIED. ) ;
#16918 = VERTEX_POINT ( 'NONE', #2772 ) ;
#16919 = CARTESIAN_POINT ( 'NONE',  ( 2.636624412717099908, 15.80357026013547816, -2.862162146981609201 ) ) ;
#16920 = ADVANCED_FACE ( 'NONE', ( #7681 ), #589, .F. ) ;
#16921 = CARTESIAN_POINT ( 'NONE',  ( 1.977436885025663837, -15.04044112860237625, 3.321781585408698056 ) ) ;
#16922 = LINE ( 'NONE', #871, #4253 ) ;
#16923 =( BOUNDED_SURFACE ( )  B_SPLINE_SURFACE ( 3, 1, ( 
 ( #9574, #520 ),
 ( #13876, #17914 ),
 ( #5089, #4996 ),
 ( #4819, #10838 ) ),
 .UNSPECIFIED., .F., .F., .T. ) 
 B_SPLINE_SURFACE_WITH_KNOTS ( ( 4, 4 ),
 ( 2, 2 ),
 ( 0.000000000000000000, 1.000000000000000000 ),
 ( 0.000000000000000000, 1.000000000000000000 ),
 .UNSPECIFIED. ) 
 GEOMETRIC_REPRESENTATION_ITEM ( )  RATIONAL_B_SPLINE_SURFACE ( (
 ( 1.000000000000000000, 1.000000000000000000),
 ( 0.9933953342250436691, 0.8357391271907733676),
 ( 0.9933953342250436691, 0.8357391271907733676),
 ( 1.000000000000000000, 1.000000000000000000) ) ) 
 REPRESENTATION_ITEM ( '' )  SURFACE ( )  );
#16924 =( BOUNDED_SURFACE ( )  B_SPLINE_SURFACE ( 3, 1, ( 
 ( #6515, #12334 ),
 ( #14051, #5068 ),
 ( #15295, #955 ),
 ( #2208, #8049 ) ),
 .UNSPECIFIED., .F., .F., .F. ) 
 B_SPLINE_SURFACE_WITH_KNOTS ( ( 4, 4 ),
 ( 2, 2 ),
 ( 0.000000000000000000, 1.000000000000000000 ),
 ( 0.000000000000000000, 1.000000000000000000 ),
 .UNSPECIFIED. ) 
 GEOMETRIC_REPRESENTATION_ITEM ( )  RATIONAL_B_SPLINE_SURFACE ( (
 ( 1.000000000000000000, 1.000000000000000000),
 ( 0.9933953342250438912, 0.8357391271907739227),
 ( 0.9933953342250438912, 0.8357391271907739227),
 ( 1.000000000000000000, 1.000000000000000000) ) ) 
 REPRESENTATION_ITEM ( '' )  SURFACE ( )  );
#16925 = CARTESIAN_POINT ( 'NONE',  ( 1.846955891736115518, 9.909315188408152508, -7.525208385419853485 ) ) ;
#16926 = DIRECTION ( 'NONE',  ( 0.000000000000000000, -1.000000000000000000, 0.000000000000000000 ) ) ;
#16927 = CIRCLE ( 'NONE', #5369, 2.600000000000039613 ) ;
#16928 = VECTOR ( 'NONE', #2008, 1000.000000000000000 ) ;
#16929 = CARTESIAN_POINT ( 'NONE',  ( 8.438534575730034959, -3.845978796785994192, -5.688336279099088344 ) ) ;
#16930 = VECTOR ( 'NONE', #18881, 1000.000000000000000 ) ;
#16931 = DIRECTION ( 'NONE',  ( 1.000000000000000000, 0.000000000000000000, 0.000000000000000000 ) ) ;
#16933 = ORIENTED_EDGE ( 'NONE', *, *, #17349, .F. ) ;
#16932 = CARTESIAN_POINT ( 'NONE',  ( 15.00000000000000711, -15.99999999999999645, 8.000000000000000000 ) ) ;
#16934 = CARTESIAN_POINT ( 'NONE',  ( 16.57778382496167424, -0.01466529584256673520, 0.002851818597093359019 ) ) ;
#16935 = B_SPLINE_CURVE_WITH_KNOTS ( 'NONE', 3,
 ( #16802, #17145, #4056, #9872 ),
 .UNSPECIFIED., .F., .F.,
 ( 4, 4 ),
 ( 9.204257061898183523E-17, 0.002004993803842712065 ),
 .UNSPECIFIED. ) ;
#16936 = CARTESIAN_POINT ( 'NONE',  ( 2.747332970342022840, -2.409922051470567261, -16.17136872824901062 ) ) ;
#16937 = CARTESIAN_POINT ( 'NONE',  ( 0.3145729642390375225, -4.535980493005000724, -12.96842777670211611 ) ) ;
#16938 = B_SPLINE_CURVE_WITH_KNOTS ( 'NONE', 3,
 ( #12721, #2396, #18550, #5455, #17208, #8421 ),
 .UNSPECIFIED., .F., .F.,
 ( 4, 2, 4 ),
 ( 4.269227611140977934E-17, 0.0002014099069817279985, 0.0004028198139634133336 ),
 .UNSPECIFIED. ) ;
#16939 = ORIENTED_EDGE ( 'NONE', *, *, #17842, .T. ) ;
#16940 = EDGE_CURVE ( 'NONE', #12010, #2621, #16250, .T. ) ;
#16941 = ORIENTED_EDGE ( 'NONE', *, *, #10701, .T. ) ;
#16942 = FACE_OUTER_BOUND ( 'NONE', #5040, .T. ) ;
#16943 = CARTESIAN_POINT ( 'NONE',  ( 1.861706995891676764, 12.44571539481144384, -0.5394761475746276957 ) ) ;
#16944 = VECTOR ( 'NONE', #16926, 1000.000000000000000 ) ;
#16945 = ORIENTED_EDGE ( 'NONE', *, *, #5419, .F. ) ;
#16946 = CARTESIAN_POINT ( 'NONE',  ( 2.747332970342022840, -2.409922051470567261, -16.17136872824901062 ) ) ;
#16947 = VECTOR ( 'NONE', #2835, 999.9999999999998863 ) ;
#16948 = CARTESIAN_POINT ( 'NONE',  ( 2.002547531651520885, 10.57595306287292480, 6.845637710436228929 ) ) ;
#16949 = CARTESIAN_POINT ( 'NONE',  ( -194.9999999999999716, -40.00000000000003553, 0.000000000000000000 ) ) ;
#16950 = DIRECTION ( 'NONE',  ( -0.000000000000000000, -0.000000000000000000, 1.000000000000000000 ) ) ;
#16951 = CARTESIAN_POINT ( 'NONE',  ( 1.846524061778018977, 7.023652644192272199, 10.27028962889599484 ) ) ;
#16952 = SHAPE_DEFINITION_REPRESENTATION ( #368, #16816 ) ;
#16953 = FILL_AREA_STYLE ('',( #11502 ) ) ;
#16954 = CARTESIAN_POINT ( 'NONE',  ( 16.56782317627811096, 0.005492611183758417011, 0.008141063682853501640 ) ) ;
#16955 = CARTESIAN_POINT ( 'NONE',  ( 0.3150686449036028680, -13.01866258978840030, 4.391272911157273029 ) ) ;
#16956 =( REPRESENTATION_RELATIONSHIP ('NONE','NONE', #5200, #14858 ) REPRESENTATION_RELATIONSHIP_WITH_TRANSFORMATION ( #14356 )SHAPE_REPRESENTATION_RELATIONSHIP( ) );
#16957 = AXIS2_PLACEMENT_3D ( 'NONE', #10665, #6367, #7805 ) ;
#16958 = CARTESIAN_POINT ( 'NONE',  ( 0.3132635586635976188, -4.743936529203153007, -12.89236642382226172 ) ) ;
#16959 = CARTESIAN_POINT ( 'NONE',  ( 0.3058872367615230181, 13.24582953854925371, 3.664492643742809364 ) ) ;
#16960 = FACE_OUTER_BOUND ( 'NONE', #8186, .T. ) ;
#16961 = CARTESIAN_POINT ( 'NONE',  ( 0.3058872367615230181, 8.562166468153717958, 10.75034008168919009 ) ) ;
#16962 = EDGE_LOOP ( 'NONE', ( #7919, #6725, #8615, #4648 ) ) ;
#16963 = EDGE_CURVE ( 'NONE', #17568, #16417, #11913, .T. ) ;
#16964 = EDGE_CURVE ( 'NONE', #5602, #2485, #14726, .T. ) ;
#16965 = EDGE_CURVE ( 'NONE', #4894, #17234, #5071, .T. ) ;
#16966 = ORIENTED_EDGE ( 'NONE', *, *, #9893, .T. ) ;
#16967 = ORIENTED_EDGE ( 'NONE', *, *, #6443, .T. ) ;
#16968 = VERTEX_POINT ( 'NONE', #1742 ) ;
#16969 = VECTOR ( 'NONE', #16217, 1000.000000000000000 ) ;
#16970 = CARTESIAN_POINT ( 'NONE',  ( -199.9999999999999716, -30.00000000000003197, 3.000000000000000000 ) ) ;
#16971 = DIRECTION ( 'NONE',  ( 0.000000000000000000, 0.000000000000000000, -1.000000000000000000 ) ) ;
#16972 = B_SPLINE_CURVE_WITH_KNOTS ( 'NONE', 3,
 ( #10160, #15983, #8446, #5653, #2875, #8727 ),
 .UNSPECIFIED., .F., .F.,
 ( 4, 2, 4 ),
 ( 2.168404344971008868E-18, 0.001500839035891550922, 0.003001678071783099675 ),
 .UNSPECIFIED. ) ;
#16973 = DIRECTION ( 'NONE',  ( 0.000000000000000000, 0.000000000000000000, -1.000000000000000000 ) ) ;
#16974 = FACE_OUTER_BOUND ( 'NONE', #52, .T. ) ;
#16975 = CARTESIAN_POINT ( 'NONE',  ( 0.3058872367615226295, -10.75034008168909416, -8.562166468153835197 ) ) ;
#16976 = FACE_OUTER_BOUND ( 'NONE', #6280, .T. ) ;
#16977 = CARTESIAN_POINT ( 'NONE',  ( 16.57210152137263393, 0.009075239946109033701, 0.01136813053532163831 ) ) ;
#16978 = CARTESIAN_POINT ( 'NONE',  ( 0.3095370825347234511, 12.91933430393608084, 4.681152801286207144 ) ) ;
#16979 = EDGE_LOOP ( 'NONE', ( #13814, #18095 ) ) ;
#16980 = CIRCLE ( 'NONE', #5339, 5.000000000000000888 ) ;
#16981 = STYLED_ITEM ( 'NONE', ( #3058 ), #9004 ) ;
#16982 = ORIENTED_EDGE ( 'NONE', *, *, #3475, .F. ) ;
#16983 = ORIENTED_EDGE ( 'NONE', *, *, #3550, .F. ) ;
#16984 = VERTEX_POINT ( 'NONE', #3151 ) ;
#16985 = FACE_OUTER_BOUND ( 'NONE', #15843, .T. ) ;
#16986 = EDGE_CURVE ( 'NONE', #15892, #14167, #7387, .T. ) ;
#16987 = AXIS2_PLACEMENT_3D ( 'NONE', #11956, #5822, #12053 ) ;
#16988 = PLANE ( 'NONE',  #9327 ) ;
#16989 = CARTESIAN_POINT ( 'NONE',  ( 2.697797270744667131, -4.970631985779678352, 12.33058466479267778 ) ) ;
#16990 = CARTESIAN_POINT ( 'NONE',  ( 3.950837973638676281, 1.958075594453990487, -14.41405733518058341 ) ) ;
#16991 = CARTESIAN_POINT ( 'NONE',  ( -5.000000000000000000, 20.00000000000000000, 7.000000000000000000 ) ) ;
#16992 = EDGE_CURVE ( 'NONE', #5926, #4785, #18323, .T. ) ;
#16993 = VERTEX_POINT ( 'NONE', #4610 ) ;
#16994 = CARTESIAN_POINT ( 'NONE',  ( 2.636624412714237309, 15.91454522070173638, -2.161493821596664144 ) ) ;
#16995 = AXIS2_PLACEMENT_3D ( 'NONE', #7060, #18700, #8579 ) ;
#16996 = VECTOR ( 'NONE', #6323, 1000.000000000000000 ) ;
#16997 = CARTESIAN_POINT ( 'NONE',  ( 1.845756295923353330, 0.4783934145702027352, 12.43231724724607190 ) ) ;
#16998 = CARTESIAN_POINT ( 'NONE',  ( 0.3372494957990315734, 7.499999999999999112, -14.22369192593357923 ) ) ;
#16999 = CARTESIAN_POINT ( 'NONE',  ( 2.002547531651519996, -3.242439124566736997, 12.17374746633577232 ) ) ;
#17000 = CIRCLE ( 'NONE', #4495, 13.42403576283810906 ) ;
#17001 = EDGE_CURVE ( 'NONE', #2287, #9336, #11434, .T. ) ;
#17002 = CYLINDRICAL_SURFACE ( 'NONE', #15727, 5.000000000000000888 ) ;
#17003 = CARTESIAN_POINT ( 'NONE',  ( 0.3137051932979809665, -4.679953077377580151, 12.91601973349268917 ) ) ;
#17004 = CARTESIAN_POINT ( 'NONE',  ( 19.99999999999999645, 20.00000000000000000, 3.000000000000000000 ) ) ;
#17005 =( BOUNDED_SURFACE ( )  B_SPLINE_SURFACE ( 3, 1, ( 
 ( #15206, #13947 ),
 ( #4889, #5064 ),
 ( #10911, #2117 ),
 ( #6602, #13764 ) ),
 .UNSPECIFIED., .F., .F., .T. ) 
 B_SPLINE_SURFACE_WITH_KNOTS ( ( 4, 4 ),
 ( 2, 2 ),
 ( 0.000000000000000000, 1.000000000000000000 ),
 ( 0.000000000000000000, 1.000000000000000000 ),
 .UNSPECIFIED. ) 
 GEOMETRIC_REPRESENTATION_ITEM ( )  RATIONAL_B_SPLINE_SURFACE ( (
 ( 1.000000000000000000, 1.000000000000000000),
 ( 0.7792777138730158093, 0.9689936506012928330),
 ( 0.7792777138730158093, 0.9689936506012928330),
 ( 1.000000000000000000, 1.000000000000000000) ) ) 
 REPRESENTATION_ITEM ( '' )  SURFACE ( )  );
#17006 = CARTESIAN_POINT ( 'NONE',  ( -4.000000000000000888, 17.00000000000000000, 8.000000000000000000 ) ) ;
#17007 = EDGE_LOOP ( 'NONE', ( #13024, #12884, #9793, #5907 ) ) ;
#17008 = AXIS2_PLACEMENT_3D ( 'NONE', #13025, #1368, #28 ) ;
#17010 = ORIENTED_EDGE ( 'NONE', *, *, #7530, .T. ) ;
#17009 = DIRECTION ( 'NONE',  ( -1.000000000000000000, -0.000000000000000000, -0.000000000000000000 ) ) ;
#17011 = CIRCLE ( 'NONE', #13662, 1.000000000000000000 ) ;
#17012 = VECTOR ( 'NONE', #7892, 1000.000000000000000 ) ;
#17013 = B_SPLINE_CURVE_WITH_KNOTS ( 'NONE', 3,
 ( #13578, #498, #4870, #2552, #1135, #3916 ),
 .UNSPECIFIED., .F., .F.,
 ( 4, 2, 4 ),
 ( 0.000000000000000000, 0.001656992708822042004, 0.003313985417644083140 ),
 .UNSPECIFIED. ) ;
#17014 = EDGE_CURVE ( 'NONE', #9580, #15726, #6337, .T. ) ;
#17015 = CARTESIAN_POINT ( 'NONE',  ( -2.750000000000000000, 3.367778697655221012E-16, 11.00000000000000000 ) ) ;
#17016 = VERTEX_POINT ( 'NONE', #507 ) ;
#17017 = DIRECTION ( 'NONE',  ( -1.000000000000000000, -0.000000000000000000, -0.000000000000000000 ) ) ;
#17018 = EDGE_CURVE ( 'NONE', #4102, #8021, #3684, .T. ) ;
#17019 = EDGE_CURVE ( 'NONE', #18802, #10356, #285, .T. ) ;
#17020 = CARTESIAN_POINT ( 'NONE',  ( -5.029793280284183155, -7.500000000000000888, -16.81208494724225133 ) ) ;
#17021 = CARTESIAN_POINT ( 'NONE',  ( 3.950837973638668288, 0.000000000000000000, 0.000000000000000000 ) ) ;
#17022 = EDGE_LOOP ( 'NONE', ( #1316, #18028, #2031, #15936 ) ) ;
#17023 = CARTESIAN_POINT ( 'NONE',  ( 1.847034903785828019, -7.498375632854680006, 9.929438108952115982 ) ) ;
#17024 = CARTESIAN_POINT ( 'NONE',  ( 0.3132642857406535697, -13.21852905223341601, 3.740125687984681591 ) ) ;
#17025 = CARTESIAN_POINT ( 'NONE',  ( 1.847461586945730483, 12.44326124954594626, -0.03350899125597195383 ) ) ;
#17026 = DIRECTION ( 'NONE',  ( 0.000000000000000000, -1.000000000000000000, 0.000000000000000000 ) ) ;
#17027 = FACE_OUTER_BOUND ( 'NONE', #17566, .T. ) ;
#17028 = EDGE_CURVE ( 'NONE', #9866, #2315, #6141, .T. ) ;
#17029 = CARTESIAN_POINT ( 'NONE',  ( 1.342453679581834924, -13.74702459364888263, 5.476372339889963747 ) ) ;
#17030 = FACE_BOUND ( 'NONE', #7101, .T. ) ;
#17032 = ORIENTED_EDGE ( 'NONE', *, *, #15576, .T. ) ;
#17031 = CARTESIAN_POINT ( 'NONE',  ( 0.4862570985993235340, 5.003653737315670647, -12.97920246947874112 ) ) ;
#17033 = CARTESIAN_POINT ( 'NONE',  ( 0.8740779401512712710, 11.05257166392075341, -9.070947476926923159 ) ) ;
#17034 = AXIS2_PLACEMENT_3D ( 'NONE', #17225, #18383, #15603 ) ;
#17035 = CARTESIAN_POINT ( 'NONE',  ( 0.3150686449036049219, -13.11344473514185971, -4.099563462784791668 ) ) ;
#17036 = ORIENTED_EDGE ( 'NONE', *, *, #8834, .T. ) ;
#17037 = LINE ( 'NONE', #18643, #9353 ) ;
#17038 = DIRECTION ( 'NONE',  ( 0.000000000000000000, 0.000000000000000000, 1.000000000000000000 ) ) ;
#17039 =( BOUNDED_SURFACE ( )  B_SPLINE_SURFACE ( 3, 1, ( 
 ( #18736, #1449 ),
 ( #1162, #11490 ),
 ( #2765, #1347 ),
 ( #13105, #14260 ) ),
 .UNSPECIFIED., .F., .F., .T. ) 
 B_SPLINE_SURFACE_WITH_KNOTS ( ( 4, 4 ),
 ( 2, 2 ),
 ( 0.000000000000000000, 1.000000000000000000 ),
 ( 0.000000000000000000, 1.000000000000000000 ),
 .UNSPECIFIED. ) 
 GEOMETRIC_REPRESENTATION_ITEM ( )  RATIONAL_B_SPLINE_SURFACE ( (
 ( 1.000000000000000000, 1.000000000000000000),
 ( 0.9933953342250436691, 0.8357391271907733676),
 ( 0.9933953342250436691, 0.8357391271907733676),
 ( 1.000000000000000000, 1.000000000000000000) ) ) 
 REPRESENTATION_ITEM ( '' )  SURFACE ( )  );
#17040 = ORIENTED_EDGE ( 'NONE', *, *, #15246, .T. ) ;
#17041 = CARTESIAN_POINT ( 'NONE',  ( 0.3939822652208148646, -4.930560016699156556, 12.90851734139305229 ) ) ;
#17042 = CARTESIAN_POINT ( 'NONE',  ( 0.3308579732647018989, 11.46737410776364996, -7.595989242675004860 ) ) ;
#17043 = DIRECTION ( 'NONE',  ( 0.000000000000000000, 0.000000000000000000, -1.000000000000000000 ) ) ;
#17044 = UNCERTAINTY_MEASURE_WITH_UNIT (LENGTH_MEASURE( 1.000000000000000082E-05 ), #2448, 'distance_accuracy_value', 'NONE');
#17045 = APPLICATION_PROTOCOL_DEFINITION ( 'draft international standard', 'automotive_design', 1998, #13881 ) ;
#17046 =( LENGTH_UNIT ( ) NAMED_UNIT ( * ) SI_UNIT ( .MILLI., .METRE. ) );
#17047 = CARTESIAN_POINT ( 'NONE',  ( 5.000000000000000000, 0.000000000000000000, 7.000000000000000000 ) ) ;
#17048 = ADVANCED_FACE ( 'NONE', ( #10535 ), #16372, .F. ) ;
#17049 = CARTESIAN_POINT ( 'NONE',  ( 0.000000000000000000, 0.000000000000000000, 0.000000000000000000 ) ) ;
#17050 = CARTESIAN_POINT ( 'NONE',  ( 2.705023505549867924, -0.8488853074252048492, -13.27418276223637150 ) ) ;
#17051 = CARTESIAN_POINT ( 'NONE',  ( 0.3095370825347224519, 11.38092634279639626, -7.700448427571749299 ) ) ;
#17052 = DIRECTION ( 'NONE',  ( 0.000000000000000000, 0.000000000000000000, 1.000000000000000000 ) ) ;
#17053 = CARTESIAN_POINT ( 'NONE',  ( 1.846138399168762101, 12.43476674860266584, -0.4167076046095982700 ) ) ;
#17054 = CARTESIAN_POINT ( 'NONE',  ( 1.845756295923353996, 6.920504327368345976, -10.33914852636097592 ) ) ;
#17055 = ORIENTED_EDGE ( 'NONE', *, *, #700, .T. ) ;
#17056 = ORIENTED_EDGE ( 'NONE', *, *, #9985, .T. ) ;
#17057 = VERTEX_POINT ( 'NONE', #602 ) ;
#17058 = ORIENTED_EDGE ( 'NONE', *, *, #1206, .T. ) ;
#17059 = CARTESIAN_POINT ( 'NONE',  ( 1.847426409206450959, 1.966388007708274189E-11, -12.44303504652081038 ) ) ;
#17060 = DIRECTION ( 'NONE',  ( -1.000000000000000000, 0.000000000000000000, 0.000000000000000000 ) ) ;
#17061 = B_SPLINE_CURVE_WITH_KNOTS ( 'NONE', 3,
 ( #11901, #8642, #5667, #18868, #4348, #14568 ),
 .UNSPECIFIED., .F., .F.,
 ( 4, 2, 4 ),
 ( 0.000000000000000000, 0.001657017934712276541, 0.003314035869424553082 ),
 .UNSPECIFIED. ) ;
#17062 = DIRECTION ( 'NONE',  ( -0.7561779333270775005, 0.6322161072786942615, 0.1688126975276577901 ) ) ;
#17063 = CARTESIAN_POINT ( 'NONE',  ( 1.560000000000000053, -0.8660254037844384856, -1.500000000000000000 ) ) ;
#17064 = EDGE_CURVE ( 'NONE', #4298, #14216, #3326, .T. ) ;
#17065 = FILL_AREA_STYLE ('',( #8369 ) ) ;
#17066 = ADVANCED_FACE ( 'NONE', ( #18176 ), #2213, .T. ) ;
#17067 = FACE_OUTER_BOUND ( 'NONE', #2227, .T. ) ;
#17068 = EDGE_CURVE ( 'NONE', #3117, #14815, #18500, .T. ) ;
#17069 = CARTESIAN_POINT ( 'NONE',  ( 0.3150686449036029790, -0.1533607327084788585, -13.73846184595214481 ) ) ;
#17070 = CARTESIAN_POINT ( 'NONE',  ( 1.846138399168762989, 11.69739621335922308, 4.238866729160444713 ) ) ;
#17071 = DIRECTION ( 'NONE',  ( -1.000000000000000000, -0.000000000000000000, -0.000000000000000000 ) ) ;
#17072 = ORIENTED_EDGE ( 'NONE', *, *, #9877, .F. ) ;
#17073 = ORIENTED_EDGE ( 'NONE', *, *, #17461, .T. ) ;
#17074 = B_SPLINE_CURVE_WITH_KNOTS ( 'NONE', 3,
 ( #2317, #13978, #886, #8072, #9843, #14157 ),
 .UNSPECIFIED., .F., .F.,
 ( 4, 2, 4 ),
 ( 3.499941646806256644E-17, 0.0001825746017570586152, 0.0003651492035140799881 ),
 .UNSPECIFIED. ) ;
#17075 = PRESENTATION_LAYER_ASSIGNMENT (  '', '', ( #17705 ) ) ;
#17076 = EDGE_LOOP ( 'NONE', ( #12930, #3472, #7835, #14691 ) ) ;
#17077 = ORIENTED_EDGE ( 'NONE', *, *, #440, .T. ) ;
#17078 = EDGE_CURVE ( 'NONE', #5504, #256, #10034, .T. ) ;
#17079 = DIRECTION ( 'NONE',  ( -1.000000000000000000, -0.000000000000000000, -0.000000000000000000 ) ) ;
#17080 = CARTESIAN_POINT ( 'NONE',  ( 3.664313757352971823, -13.97913389346635427, 2.831308606787193316 ) ) ;
#17081 = CARTESIAN_POINT ( 'NONE',  ( 1.845756295923356438, -11.67600463554276224, 4.296776483139434610 ) ) ;
#17082 = CARTESIAN_POINT ( 'NONE',  ( 0.3137051932979775248, 10.83767969834815581, -8.442169467526731808 ) ) ;
#17083 = CARTESIAN_POINT ( 'NONE',  ( 1.847412631396503357, -7.348689888531914072, 10.04119192206683664 ) ) ;
#17084 = ORIENTED_EDGE ( 'NONE', *, *, #15352, .T. ) ;
#17085 = DIRECTION ( 'NONE',  ( -0.9034263296138842492, 0.000000000000000000, -0.4287433579198461908 ) ) ;
#17086 = CARTESIAN_POINT ( 'NONE',  ( 1.847461586945727596, -11.84459954310608332, -3.813310247068566028 ) ) ;
#17087 = CARTESIAN_POINT ( 'NONE',  ( 3.253466017773726904, 7.500000000000133227, -13.21345932477064622 ) ) ;
#17088 = CARTESIAN_POINT ( 'NONE',  ( 0.3132642857406528480, 13.72733058964895037, 0.5276792104582755938 ) ) ;
#17089 = CARTESIAN_POINT ( 'NONE',  ( 0.4862570985993252548, 13.44146924561381162, 3.580942890621718888 ) ) ;
#17090 = CARTESIAN_POINT ( 'NONE',  ( 1.861628059977343597, -10.38573835516717381, 6.879051339207257421 ) ) ;
#17091 = FACE_OUTER_BOUND ( 'NONE', #5735, .T. ) ;
#17092 = CARTESIAN_POINT ( 'NONE',  ( 2.353870697619111052, 4.720869121224300358, -12.05847592522638934 ) ) ;
#17093 = VERTEX_POINT ( 'NONE', #12521 ) ;
#17094 = EDGE_CURVE ( 'NONE', #16055, #3103, #14402, .T. ) ;
#17096 = ORIENTED_EDGE ( 'NONE', *, *, #4769, .T. ) ;
#17095 = DIRECTION ( 'NONE',  ( 0.000000000000000000, 0.000000000000000000, 1.000000000000000000 ) ) ;
#17097 = CARTESIAN_POINT ( 'NONE',  ( 1.342453679581834924, 14.34050741580207067, 3.649820028552781093 ) ) ;
#17098 = FACE_OUTER_BOUND ( 'NONE', #13605, .T. ) ;
#17099 = EDGE_CURVE ( 'NONE', #11392, #5432, #2745, .T. ) ;
#17100 = ORIENTED_EDGE ( 'NONE', *, *, #1975, .F. ) ;
#17101 = CARTESIAN_POINT ( 'NONE',  ( 2.697797270744669351, 3.226410068829429711, 12.89731672021091846 ) ) ;
#17102 = CARTESIAN_POINT ( 'NONE',  ( 0.000000000000000000, 0.000000000000000000, -3.000000000000000000 ) ) ;
#17103 = DIRECTION ( 'NONE',  ( 0.000000000000000000, -1.000000000000000000, 0.000000000000000000 ) ) ;
#17104 = CARTESIAN_POINT ( 'NONE',  ( 16.56753206892534891, -0.008490833999798953410, -0.004253784598196148035 ) ) ;
#17105 = ORIENTED_EDGE ( 'NONE', *, *, #12795, .F. ) ;
#17106 = CARTESIAN_POINT ( 'NONE',  ( -7.000000000000000000, 8.572527594031473190E-16, -12.00000000000000000 ) ) ;
#17107 = CARTESIAN_POINT ( 'NONE',  ( 2.002547531651519996, 3.242439124566821818, -12.17374746633574745 ) ) ;
#17108 = CARTESIAN_POINT ( 'NONE',  ( 0.3939822652208129217, -13.80035637018650974, -0.7002900021919380436 ) ) ;
#17109 = DIRECTION ( 'NONE',  ( -1.000000000000000000, -0.000000000000000000, -0.000000000000000000 ) ) ;
#17110 =( BOUNDED_SURFACE ( )  B_SPLINE_SURFACE ( 3, 1, ( 
 ( #8073, #3663 ),
 ( #18102, #7898 ),
 ( #13882, #9579 ),
 ( #12540, #13708 ) ),
 .UNSPECIFIED., .F., .F., .T. ) 
 B_SPLINE_SURFACE_WITH_KNOTS ( ( 4, 4 ),
 ( 2, 2 ),
 ( 0.000000000000000000, 1.000000000000000000 ),
 ( 0.000000000000000000, 1.000000000000000000 ),
 .UNSPECIFIED. ) 
 GEOMETRIC_REPRESENTATION_ITEM ( )  RATIONAL_B_SPLINE_SURFACE ( (
 ( 1.000000000000000000, 1.000000000000000000),
 ( 0.9933953342250438912, 0.8357391271907739227),
 ( 0.9933953342250438912, 0.8357391271907739227),
 ( 1.000000000000000000, 1.000000000000000000) ) ) 
 REPRESENTATION_ITEM ( '' )  SURFACE ( )  );
#17111 = DIRECTION ( 'NONE',  ( -1.000000000000000000, -0.000000000000000000, -0.000000000000000000 ) ) ;
#17112 = CARTESIAN_POINT ( 'NONE',  ( 2.949999999999999734, 0.000000000000000000, 2.699999999999999734 ) ) ;
#17113 = LINE ( 'NONE', #11209, #7065 ) ;
#17115 = ORIENTED_EDGE ( 'NONE', *, *, #13090, .F. ) ;
#17114 = CARTESIAN_POINT ( 'NONE',  ( 0.000000000000000000, 0.000000000000000000, 0.000000000000000000 ) ) ;
#17116 = FACE_BOUND ( 'NONE', #5870, .T. ) ;
#17117 = CARTESIAN_POINT ( 'NONE',  ( 0.000000000000000000, 2.375000000000000444, 0.000000000000000000 ) ) ;
#17118 = EDGE_CURVE ( 'NONE', #8066, #7506, #6699, .T. ) ;
#17119 = ORIENTED_EDGE ( 'NONE', *, *, #10490, .T. ) ;
#17120 = DIRECTION ( 'NONE',  ( 0.000000000000000000, 0.000000000000000000, 1.000000000000000000 ) ) ;
#17121 = CARTESIAN_POINT ( 'NONE',  ( 2.320521194583477165, -6.542541239686160637, -14.32454473829993447 ) ) ;
#17122 = ORIENTED_EDGE ( 'NONE', *, *, #13531, .F. ) ;
#17123 = CARTESIAN_POINT ( 'NONE',  ( 1.959283090834856633, -0.6676170829051342182, -12.53713130127478692 ) ) ;
#17124 = EDGE_CURVE ( 'NONE', #16555, #7666, #1221, .T. ) ;
#17125 = DIRECTION ( 'NONE',  ( 1.000000000000000000, -0.000000000000000000, -0.000000000000000000 ) ) ;
#17126 = AXIS2_PLACEMENT_3D ( 'NONE', #14593, #1512, #17858 ) ;
#17127 = CARTESIAN_POINT ( 'NONE',  ( 1.847247051441587518, -9.967131402978145260, -7.448813758297282206 ) ) ;
#17128 = CARTESIAN_POINT ( 'NONE',  ( 1.959212340397946450, 7.909199412631302550, -9.750290364083546990 ) ) ;
#17129 = CARTESIAN_POINT ( 'NONE',  ( 16.56753206892534891, 0.008432171035096448775, -0.004368917149005366145 ) ) ;
#17130 = ORIENTED_EDGE ( 'NONE', *, *, #8833, .T. ) ;
#17131 = CONTEXT_DEPENDENT_SHAPE_REPRESENTATION ( #18899, #13165 ) ;
#17132 = SURFACE_SIDE_STYLE ('',( #17320 ) ) ;
#17133 = FACE_OUTER_BOUND ( 'NONE', #729, .T. ) ;
#17134 = CARTESIAN_POINT ( 'NONE',  ( -199.9999999999999716, -5.000000000000024869, 6.000000000000000000 ) ) ;
#17135 = CARTESIAN_POINT ( 'NONE',  ( -32.49999999999999289, -12.50000000000000178, 6.000000000000000000 ) ) ;
#17136 = FACE_OUTER_BOUND ( 'NONE', #2906, .T. ) ;
#17137 = FACE_OUTER_BOUND ( 'NONE', #15207, .T. ) ;
#17138 = VERTEX_POINT ( 'NONE', #16744 ) ;
#17139 = CARTESIAN_POINT ( 'NONE',  ( 0.3151926232592440202, 11.07013665200807395, -8.137833541809259330 ) ) ;
#17140 = CARTESIAN_POINT ( 'NONE',  ( 2.747332970342022840, -7.289199830147212289, 14.63517873738944708 ) ) ;
#17141 = EDGE_LOOP ( 'NONE', ( #5253, #16233, #4511, #7217 ) ) ;
#17142 = EDGE_CURVE ( 'NONE', #6611, #16284, #13015, .T. ) ;
#17143 = VERTEX_POINT ( 'NONE', #11200 ) ;
#17144 = ORIENTED_EDGE ( 'NONE', *, *, #10921, .T. ) ;
#17145 = CARTESIAN_POINT ( 'NONE',  ( 3.074695600507423521, -10.75417554975728329, -11.23985886659437483 ) ) ;
#17146 = CIRCLE ( 'NONE', #4020, 12.15840553252917289 ) ;
#17147 = EDGE_LOOP ( 'NONE', ( #17802, #7887 ) ) ;
#17148 = EDGE_CURVE ( 'NONE', #14004, #5097, #16209, .T. ) ;
#17149 = DIRECTION ( 'NONE',  ( -0.000000000000000000, 1.000000000000000000, 0.000000000000000000 ) ) ;
#17150 = CARTESIAN_POINT ( 'NONE',  ( 0.4754618798421162973, -10.80499583390506224, -8.775436892861234739 ) ) ;
#17151 = CARTESIAN_POINT ( 'NONE',  ( -30.00000000000000355, -12.50000000000000178, 6.500000000000000888 ) ) ;
#17152 = CARTESIAN_POINT ( 'NONE',  ( 0.000000000000000000, 0.000000000000000000, 8.000000000000000000 ) ) ;
#17153 = DIRECTION ( 'NONE',  ( -1.000000000000000000, -1.734723475976807094E-16, 0.000000000000000000 ) ) ;
#17154 = CARTESIAN_POINT ( 'NONE',  ( 16.57210152137263393, -0.01453130299868521901, -0.0006600038696347544425 ) ) ;
#17155 = CIRCLE ( 'NONE', #4034, 14.54644660717763927 ) ;
#17156 = LINE ( 'NONE', #14199, #6222 ) ;
#17157 = CARTESIAN_POINT ( 'NONE',  ( 1.845756295923360435, -12.43231724724606835, 0.4783934145701590479 ) ) ;
#17158 = EDGE_LOOP ( 'NONE', ( #1497, #4023, #1632, #995 ) ) ;
#17159 = ORIENTED_EDGE ( 'NONE', *, *, #2351, .T. ) ;
#17160 = ORIENTED_EDGE ( 'NONE', *, *, #16604, .T. ) ;
#17161 = EDGE_LOOP ( 'NONE', ( #18138, #3067, #13953, #17516 ) ) ;
#17162 = B_SPLINE_CURVE_WITH_KNOTS ( 'NONE', 3,
 ( #5430, #4194, #5698, #2823, #4090, #8672, #2546, #8395, #11550, #10008, #1412, #1029, #5601 ),
 .UNSPECIFIED., .F., .F.,
 ( 4, 3, 3, 3, 4 ),
 ( 2.168404344971008868E-18, 0.0002299804304191472269, 0.0004599608082120226239, 0.0006467586077647999570, 0.0008336169836825976396 ),
 .UNSPECIFIED. ) ;
#17163 = EDGE_CURVE ( 'NONE', #6853, #10307, #16922, .T. ) ;
#17164 = DIRECTION ( 'NONE',  ( 0.000000000000000000, -1.000000000000000000, 0.000000000000000000 ) ) ;
#17165 = CARTESIAN_POINT ( 'NONE',  ( 2.353870697619111940, -12.53036919722786813, 3.268530966681581607 ) ) ;
#17166 = DIRECTION ( 'NONE',  ( -1.000000000000000000, 0.000000000000000000, 0.000000000000000000 ) ) ;
#17167 = LINE ( 'NONE', #15923, #10888 ) ;
#17168 =( NAMED_UNIT ( * ) SI_UNIT ( $, .STERADIAN. ) SOLID_ANGLE_UNIT ( ) );
#17169 = ORIENTED_EDGE ( 'NONE', *, *, #5905, .T. ) ;
#17170 = FACE_OUTER_BOUND ( 'NONE', #14255, .T. ) ;
#17171 = DIRECTION ( 'NONE',  ( -0.7561779333270775005, -0.3559159372837353286, 0.5491072561318327550 ) ) ;
#17172 = LINE ( 'NONE', #4084, #18302 ) ;
#17173 = CARTESIAN_POINT ( 'NONE',  ( 0.4862570985993235340, -13.44146924561378498, -3.580942890621813923 ) ) ;
#17174 = AXIS2_PLACEMENT_3D ( 'NONE', #6478, #16703, #12303 ) ;
#17175 = CARTESIAN_POINT ( 'NONE',  ( 16.58200780006414732, -0.006043560077721775101, 0.009393638146078504489 ) ) ;
#17176 = DIRECTION ( 'NONE',  ( 0.000000000000000000, 0.000000000000000000, -1.000000000000000000 ) ) ;
#17177 = CARTESIAN_POINT ( 'NONE',  ( 0.3939822652208163078, 4.930560016699244485, -12.90851734139301499 ) ) ;
#17178 = CARTESIAN_POINT ( 'NONE',  ( 3.950837973638668288, 0.000000000000000000, 0.000000000000000000 ) ) ;
#17179 = ORIENTED_EDGE ( 'NONE', *, *, #4447, .F. ) ;
#17181 = VERTEX_POINT ( 'NONE', #6615 ) ;
#17180 = CARTESIAN_POINT ( 'NONE',  ( 2.369999999999999662, 0.000000000000000000, 0.000000000000000000 ) ) ;
#17182 = CARTESIAN_POINT ( 'NONE',  ( 2.123976203522053741, 15.26039569100260174, 3.347755036805956763 ) ) ;
#17183 = ORIENTED_EDGE ( 'NONE', *, *, #17240, .T. ) ;
#17184 = VECTOR ( 'NONE', #10262, 1000.000000000000000 ) ;
#17185 = CARTESIAN_POINT ( 'NONE',  ( 0.3720661004400040439, -10.73619472937708252, 8.694226082900557984 ) ) ;
#17186 = EDGE_CURVE ( 'NONE', #618, #8134, #9138, .T. ) ;
#17187 = VECTOR ( 'NONE', #16474, 1000.000000000000000 ) ;
#17188 = EDGE_CURVE ( 'NONE', #15164, #14390, #7800, .T. ) ;
#17189 = CIRCLE ( 'NONE', #18708, 5.000000000000049738 ) ;
#17190 = ORIENTED_EDGE ( 'NONE', *, *, #15086, .T. ) ;
#17191 = EDGE_CURVE ( 'NONE', #14815, #18903, #4871, .T. ) ;
#17192 = CARTESIAN_POINT ( 'NONE',  ( 3.950837973638676281, 13.10350451991840615, 6.316429227969512894 ) ) ;
#17193 = CARTESIAN_POINT ( 'NONE',  ( -6.499600586846986161, -2.601338725571163302, -12.00000000000000000 ) ) ;
#17194 = FACE_OUTER_BOUND ( 'NONE', #16136, .T. ) ;
#17195 = CARTESIAN_POINT ( 'NONE',  ( 3.512766787570690497, 2.682019731918607430, -14.81029789862162893 ) ) ;
#17196 = ORIENTED_EDGE ( 'NONE', *, *, #11235, .F. ) ;
#17197 = CARTESIAN_POINT ( 'NONE',  ( 1.861628059977344041, 0.5393144007391995620, -12.44564375541076551 ) ) ;
#17198 = LINE ( 'NONE', #8508, #13235 ) ;
#17199 = CARTESIAN_POINT ( 'NONE',  ( 0.3145729642390355796, -13.73540280162741212, 0.3065092323350734893 ) ) ;
#17200 = CARTESIAN_POINT ( 'NONE',  ( 0.000000000000000000, 0.000000000000000000, 8.000000000000000000 ) ) ;
#17201 = DIRECTION ( 'NONE',  ( -0.000000000000000000, 1.000000000000000000, -0.000000000000000000 ) ) ;
#17202 =( LENGTH_UNIT ( ) NAMED_UNIT ( * ) SI_UNIT ( .MILLI., .METRE. ) );
#17203 = CARTESIAN_POINT ( 'NONE',  ( 0.000000000000000000, 6.123233995736766282E-16, -5.000000000000000000 ) ) ;
#17204 = VECTOR ( 'NONE', #8032, 1000.000000000000114 ) ;
#17205 = PLANE ( 'NONE',  #15911 ) ;
#17207 = ORIENTED_EDGE ( 'NONE', *, *, #9626, .T. ) ;
#17206 = DIRECTION ( 'NONE',  ( 0.000000000000000000, 0.000000000000000000, -1.000000000000000000 ) ) ;
#17208 = CARTESIAN_POINT ( 'NONE',  ( 0.3132642857406495174, 0.5276792104584192566, -13.72733058964894681 ) ) ;
#17209 = CARTESIAN_POINT ( 'NONE',  ( 1.254009781011619751, -13.61532727684435251, 5.487405433548490308 ) ) ;
#17210 = ORIENTED_EDGE ( 'NONE', *, *, #9146, .F. ) ;
#17211 = CARTESIAN_POINT ( 'NONE',  ( 0.3137051932979792457, 4.679953077377670745, -12.91601973349265720 ) ) ;
#17212 = CARTESIAN_POINT ( 'NONE',  ( 0.3151928479966097374, 0.000000000000000000, -13.73922861026898623 ) ) ;
#17213 = ORIENTED_EDGE ( 'NONE', *, *, #12847, .T. ) ;
#17214 = CARTESIAN_POINT ( 'NONE',  ( 16.56679352167444819, -0.009190982326619729845, -0.001390132774594407148 ) ) ;
#17215 = EDGE_CURVE ( 'NONE', #7783, #11285, #14139, .T. ) ;
#17216 = FILL_AREA_STYLE_COLOUR ( '', #13731 ) ;
#17217 = AXIS2_PLACEMENT_3D ( 'NONE', #6305, #17873, #4585 ) ;
#17218 = EDGE_CURVE ( 'NONE', #4154, #1807, #10080, .T. ) ;
#17219 = CARTESIAN_POINT ( 'NONE',  ( -61.35602477868047799, -10.00000000000000888, 3.000000000000000000 ) ) ;
#17220 = CARTESIAN_POINT ( 'NONE',  ( 0.3150686449036029790, -0.1533607327084788585, -13.73846184595214481 ) ) ;
#17221 = DIRECTION ( 'NONE',  ( 0.7635533937278216055, 0.1790966170213880715, 0.6204116510013496510 ) ) ;
#17222 = ORIENTED_EDGE ( 'NONE', *, *, #5774, .T. ) ;
#17223 = ITEM_DEFINED_TRANSFORMATION ( 'NONE', 'NONE', #10916,  #2030 ) ;
#17224 = CARTESIAN_POINT ( 'NONE',  ( 0.3137051932979792457, -13.20008686438103140, -3.805684345189927154 ) ) ;
#17225 = CARTESIAN_POINT ( 'NONE',  ( -1.979226605763932723, -14.99999999999999645, 3.000000000000000000 ) ) ;
#17226 = DIRECTION ( 'NONE',  ( -0.000000000000000000, -0.000000000000000000, -1.000000000000000000 ) ) ;
#17227 = DIRECTION ( 'NONE',  ( 0.000000000000000000, 0.000000000000000000, 1.000000000000000000 ) ) ;
#17228 = DIRECTION ( 'NONE',  ( 1.000000000000000000, 0.000000000000000000, 0.000000000000000000 ) ) ;
#17229 = AXIS2_PLACEMENT_3D ( 'NONE', #18438, #3732, #2297 ) ;
#17230 = ORIENTED_EDGE ( 'NONE', *, *, #6617, .F. ) ;
#17231 = LINE ( 'NONE', #14364, #543 ) ;
#17232 = CARTESIAN_POINT ( 'NONE',  ( 16.56872352241294521, -0.004907101719995745834, -0.009207754980064182873 ) ) ;
#17233 = AXIS2_PLACEMENT_3D ( 'NONE', #17390, #17111, #4303 ) ;
#17234 = VERTEX_POINT ( 'NONE', #12987 ) ;
#17235 = AXIS2_PLACEMENT_3D ( 'NONE', #9743, #5614, #5255 ) ;
#17236 = VERTEX_POINT ( 'NONE', #17388 ) ;
#17237 = CARTESIAN_POINT ( 'NONE',  ( 0.4754618798421167414, -13.89949764182682124, -0.7484603771385852644 ) ) ;
#17238 = ORIENTED_EDGE ( 'NONE', *, *, #16992, .T. ) ;
#17239 = CARTESIAN_POINT ( 'NONE',  ( 0.3148213771069364175, -0.2297580318215671491, 13.73693585713734144 ) ) ;
#17240 = EDGE_CURVE ( 'NONE', #8960, #5922, #14607, .T. ) ;
#17241 = ORIENTED_EDGE ( 'NONE', *, *, #7966, .T. ) ;
#17242 = EDGE_CURVE ( 'NONE', #5687, #31, #1612, .T. ) ;
#17243 = CARTESIAN_POINT ( 'NONE',  ( 3.950837973638675393, 2.591948120961804936, 14.31366178983254578 ) ) ;
#17244 = CARTESIAN_POINT ( 'NONE',  ( 0.3151930723728407768, 13.09040889075576608, -4.172946285306434078 ) ) ;
#17245 = CIRCLE ( 'NONE', #15118, 5.000000000000004441 ) ;
#17246 = CARTESIAN_POINT ( 'NONE',  ( 0.3720661004400037664, -0.7231997263365766981, 13.79610186261029448 ) ) ;
#17247 = DIRECTION ( 'NONE',  ( 0.000000000000000000, 0.000000000000000000, -1.000000000000000000 ) ) ;
#17248 = AXIS2_PLACEMENT_3D ( 'NONE', #3310, #1897, #4570 ) ;
#17249 = DIRECTION ( 'NONE',  ( 1.000000000000000000, 0.000000000000000000, 0.000000000000000000 ) ) ;
#17250 = DIRECTION ( 'NONE',  ( 1.000000000000000000, 0.000000000000000000, 0.000000000000000000 ) ) ;
#17251 = DIRECTION ( 'NONE',  ( -1.000000000000000000, -0.000000000000000000, -0.000000000000000000 ) ) ;
#17252 = EDGE_CURVE ( 'NONE', #879, #3542, #12524, .T. ) ;
#17253 = ORIENTED_EDGE ( 'NONE', *, *, #6802, .F. ) ;
#17254 = ORIENTED_EDGE ( 'NONE', *, *, #13769, .T. ) ;
#17255 = EDGE_CURVE ( 'NONE', #17352, #4785, #18046, .T. ) ;
#17256 = ORIENTED_EDGE ( 'NONE', *, *, #16341, .T. ) ;
#17257 = ORIENTED_EDGE ( 'NONE', *, *, #2128, .T. ) ;
#17258 = ORIENTED_EDGE ( 'NONE', *, *, #15444, .F. ) ;
#17259 = DIRECTION ( 'NONE',  ( -1.000000000000000000, -0.000000000000000000, -0.000000000000000000 ) ) ;
#17260 = FACE_BOUND ( 'NONE', #4788, .T. ) ;
#17261 = CARTESIAN_POINT ( 'NONE',  ( 0.3148208552358927603, 7.888357771040864996, -11.24855514421867042 ) ) ;
#17262 = ORIENTED_EDGE ( 'NONE', *, *, #6641, .T. ) ;
#17263 = CARTESIAN_POINT ( 'NONE',  ( 2.697797270744667131, 13.26309265156977624, 0.9169917281807724585 ) ) ;
#17264 = DIRECTION ( 'NONE',  ( 0.000000000000000000, 0.000000000000000000, -1.000000000000000000 ) ) ;
#17265 = CARTESIAN_POINT ( 'NONE',  ( 4.162578369387309074, 7.499999999999999112, -16.52352554129636886 ) ) ;
#17266 = LINE ( 'NONE', #10196, #14018 ) ;
#17267 = DIRECTION ( 'NONE',  ( 1.000000000000000000, -0.000000000000000000, -0.000000000000000000 ) ) ;
#17268 = CARTESIAN_POINT ( 'NONE',  ( 0.000000000000000000, 0.000000000000000000, 3.000000000000000000 ) ) ;
#17269 = DIRECTION ( 'NONE',  ( 0.000000000000000000, 0.000000000000000000, 1.000000000000000000 ) ) ;
#17270 = CONICAL_SURFACE ( 'NONE', #12397, 12.15840553252917289, 0.7853981625000049371 ) ;
#17271 = PRESENTATION_LAYER_ASSIGNMENT (  '', '', ( #16981 ) ) ;
#17272 = LINE ( 'NONE', #12784, #18259 ) ;
#17273 = EDGE_CURVE ( 'NONE', #14769, #2548, #3675, .T. ) ;
#17274 = ORIENTED_EDGE ( 'NONE', *, *, #1832, .T. ) ;
#17275 = VERTEX_POINT ( 'NONE', #2474 ) ;
#17276 = CARTESIAN_POINT ( 'NONE',  ( 0.3095370825347224519, -13.73357284481725138, 0.4597470195089713441 ) ) ;
#17277 = ORIENTED_EDGE ( 'NONE', *, *, #13873, .T. ) ;
#17278 = EDGE_LOOP ( 'NONE', ( #12859, #5881, #18319, #11509 ) ) ;
#17279 = CARTESIAN_POINT ( 'NONE',  ( 2.123976203522053297, 6.261444813538757259, -14.31368049382962937 ) ) ;
#17280 = ORIENTED_EDGE ( 'NONE', *, *, #773, .T. ) ;
#17281 = CARTESIAN_POINT ( 'NONE',  ( 1.845755665166724846, -6.920419570228271589, -10.33920510797150882 ) ) ;
#17282 = DIRECTION ( 'NONE',  ( 1.000000000000000000, 0.000000000000000000, 0.000000000000000000 ) ) ;
#17283 = CARTESIAN_POINT ( 'NONE',  ( -199.9999999999999716, 4.999999999999973355, 6.000000000000000000 ) ) ;
#17284 = CARTESIAN_POINT ( 'NONE',  ( 20.00000000000000711, -19.99999999999999645, 6.000000000000000000 ) ) ;
#17285 = EDGE_LOOP ( 'NONE', ( #18595, #1466, #13560, #8404 ) ) ;
#17286 = CARTESIAN_POINT ( 'NONE',  ( 0.4754618798421167414, -8.775436892861188554, 10.80499583390510132 ) ) ;
#17287 = AXIS2_PLACEMENT_3D ( 'NONE', #5551, #2413, #15598 ) ;
#17288 = FACE_OUTER_BOUND ( 'NONE', #839, .T. ) ;
#17289 = CARTESIAN_POINT ( 'NONE',  ( 3.950837973638676281, -14.41405733518061716, 1.958075594453740687 ) ) ;
#17290 = CARTESIAN_POINT ( 'NONE',  ( 1.846138399168762101, -6.971848976710933954, -10.30487220521577818 ) ) ;
#17291 = FACE_OUTER_BOUND ( 'NONE', #3005, .T. ) ;
#17292 = PRESENTATION_STYLE_ASSIGNMENT (( #11572 ) ) ;
#17293 = AXIS2_PLACEMENT_3D ( 'NONE', #12509, #6873, #14228 ) ;
#17294 = AXIS2_PLACEMENT_3D ( 'NONE', #4266, #17251, #11431 ) ;
#17295 = EDGE_CURVE ( 'NONE', #16918, #6853, #7559, .T. ) ;
#17296 = DIRECTION ( 'NONE',  ( 0.000000000000000000, 0.000000000000000000, 1.000000000000000000 ) ) ;
#17297 = AXIS2_PLACEMENT_3D ( 'NONE', #7695, #6901, #9672 ) ;
#17298 = CARTESIAN_POINT ( 'NONE',  ( 0.3170788640506441158, 4.100430649998145327, -13.11595226728153385 ) ) ;
#17299 = ADVANCED_FACE ( 'NONE', ( #4014 ), #9932, .T. ) ;
#17300 = EDGE_CURVE ( 'NONE', #11928, #102, #12893, .T. ) ;
#17301 = CARTESIAN_POINT ( 'NONE',  ( 1.977436885026044200, -13.27782258181834685, 7.806953934146225293 ) ) ;
#17303 = VERTEX_POINT ( 'NONE', #17289 ) ;
#17302 = CARTESIAN_POINT ( 'NONE',  ( 3.950837973638668288, 0.000000000000000000, 0.000000000000000000 ) ) ;
#17304 = CARTESIAN_POINT ( 'NONE',  ( 2.636624412715435462, -15.80357026013316712, -2.862162146983298516 ) ) ;
#17305 = EDGE_LOOP ( 'NONE', ( #8633, #8637, #18503, #6279 ) ) ;
#17306 = CARTESIAN_POINT ( 'NONE',  ( 16.56679352167444819, 0.009190982326619362083, -0.001390132774595485713 ) ) ;
#17307 = ORIENTED_EDGE ( 'NONE', *, *, #14597, .T. ) ;
#17308 = CARTESIAN_POINT ( 'NONE',  ( 1.846613052777651198, 10.26230975746759810, 7.035606253495352291 ) ) ;
#17309 = CARTESIAN_POINT ( 'NONE',  ( 0.4862570985993235340, 0.7479633556562450547, 13.89016912371017831 ) ) ;
#17310 = EDGE_CURVE ( 'NONE', #11392, #17458, #929, .T. ) ;
#17311 = VERTEX_POINT ( 'NONE', #6119 ) ;
#17312 = CARTESIAN_POINT ( 'NONE',  ( 3.950837973638676281, 6.316429227969464932, 13.10350451991842569 ) ) ;
#17313 = DIRECTION ( 'NONE',  ( -1.000000000000000000, -2.891205793294679312E-16, 0.000000000000000000 ) ) ;
#17314 = CARTESIAN_POINT ( 'NONE',  ( 0.000000000000000000, 0.000000000000000000, -13.00000000000000533 ) ) ;
#17315 = CARTESIAN_POINT ( 'NONE',  ( 0.8740764193765260259, 3.609949042658226581, 13.83508774435983035 ) ) ;
#17316 = CARTESIAN_POINT ( 'NONE',  ( 0.4754618798421162973, -13.89949764182682124, -0.7484603771385882620 ) ) ;
#17317 = ORIENTED_EDGE ( 'NONE', *, *, #12708, .F. ) ;
#17318 = ITEM_DEFINED_TRANSFORMATION ( 'NONE', 'NONE', #6015,  #2030 ) ;
#17319 = VECTOR ( 'NONE', #16879, 1000.000000000000227 ) ;
#17320 = SURFACE_STYLE_FILL_AREA ( #16953 ) ;
#17321 = CARTESIAN_POINT ( 'NONE',  ( 0.3720661004400037664, 13.34435358167257313, -3.575426119359045529 ) ) ;
#17322 = CARTESIAN_POINT ( 'NONE',  ( 3.512766787570836158, 7.127386085302768848, 13.25664064834467837 ) ) ;
#17323 = DIRECTION ( 'NONE',  ( -1.000000000000000000, 0.000000000000000000, 0.000000000000000000 ) ) ;
#17324 = DIRECTION ( 'NONE',  ( -0.000000000000000000, -0.000000000000000000, -1.000000000000000000 ) ) ;
#17325 = DIRECTION ( 'NONE',  ( -1.000000000000000000, -0.000000000000000000, -0.000000000000000000 ) ) ;
#17326 = EDGE_CURVE ( 'NONE', #15020, #18033, #17697, .T. ) ;
#17327 = EDGE_CURVE ( 'NONE', #11470, #4576, #14326, .T. ) ;
#17328 = EDGE_LOOP ( 'NONE', ( #456, #2401, #14983 ) ) ;
#17329 = FACE_OUTER_BOUND ( 'NONE', #4358, .T. ) ;
#17330 =( NAMED_UNIT ( * ) SI_UNIT ( $, .STERADIAN. ) SOLID_ANGLE_UNIT ( ) );
#17331 = ORIENTED_EDGE ( 'NONE', *, *, #17714, .T. ) ;
#17332 = VERTEX_POINT ( 'NONE', #3032 ) ;
#17333 = CARTESIAN_POINT ( 'NONE',  ( 1.847372867223026294, -0.1054171785007356615, 12.44269075185938789 ) ) ;
#17334 = ORIENTED_EDGE ( 'NONE', *, *, #1458, .F. ) ;
#17335 = CARTESIAN_POINT ( 'NONE',  ( 16.56782317627811096, 0.002708056627498641941, 0.009439921864426896805 ) ) ;
#17336 = ORIENTED_EDGE ( 'NONE', *, *, #10454, .F. ) ;
#17337 = EDGE_CURVE ( 'NONE', #8559, #17372, #605, .T. ) ;
#17338 = VECTOR ( 'NONE', #7595, 1000.000000000000000 ) ;
#17339 = CARTESIAN_POINT ( 'NONE',  ( -194.9999999999999716, 4.999999999999973355, 6.000000000000000000 ) ) ;
#17340 = CARTESIAN_POINT ( 'NONE',  ( -66.35602477868047799, 9.999999999999973355, -153.7432847437423789 ) ) ;
#17341 = CARTESIAN_POINT ( 'NONE',  ( 1.845756295923353996, 9.776763338604718356, -7.694561132136850112 ) ) ;
#17342 = CARTESIAN_POINT ( 'NONE',  ( 16.56753206892534891, 0.008490833999798002782, -0.004253784598196794220 ) ) ;
#17343 = CARTESIAN_POINT ( 'NONE',  ( 16.57210152137263393, -0.009075239946109120437, -0.01136813053532156892 ) ) ;
#17344 = CARTESIAN_POINT ( 'NONE',  ( 4.336808689942017736E-15, 0.000000000000000000, 26.00000000000000000 ) ) ;
#17345 = CARTESIAN_POINT ( 'NONE',  ( 0.3151928476913565258, -13.06671852871092199, 4.245853234426333778 ) ) ;
#17346 = CARTESIAN_POINT ( 'NONE',  ( 2.949999999999999734, 0.000000000000000000, 0.000000000000000000 ) ) ;
#17347 = ORIENTED_EDGE ( 'NONE', *, *, #6973, .F. ) ;
#17348 = ADVANCED_FACE ( 'NONE', ( #5911 ), #1717, .F. ) ;
#17349 = EDGE_CURVE ( 'NONE', #6600, #182, #484, .T. ) ;
#17350 = EDGE_LOOP ( 'NONE', ( #2997, #3634, #12447, #1976 ) ) ;
#17351 = ORIENTED_EDGE ( 'NONE', *, *, #8999, .F. ) ;
#17352 = VERTEX_POINT ( 'NONE', #2941 ) ;
#17353 = ORIENTED_EDGE ( 'NONE', *, *, #2348, .F. ) ;
#17354 = EDGE_CURVE ( 'NONE', #14283, #748, #2131, .T. ) ;
#17355 = SPHERICAL_SURFACE ( 'NONE', #12655, 5.000000000000000000 ) ;
#17356 = CARTESIAN_POINT ( 'NONE',  ( 0.3095370825347224519, 8.444334731364007141, 10.84046130709061373 ) ) ;
#17357 = CARTESIAN_POINT ( 'NONE',  ( -4.000000000000006217, 1.156482317317873500E-15, 7.000000000000000000 ) ) ;
#17358 = ORIENTED_EDGE ( 'NONE', *, *, #8624, .F. ) ;
#17359 = DIRECTION ( 'NONE',  ( 0.000000000000000000, 0.000000000000000000, 1.000000000000000000 ) ) ;
#17360 = EDGE_CURVE ( 'NONE', #5898, #4207, #5463, .T. ) ;
#17361 = CARTESIAN_POINT ( 'NONE',  ( 0.3137051932979775248, 0.4596302728639756197, 13.73004976592202198 ) ) ;
#17362 = CARTESIAN_POINT ( 'NONE',  ( 0.4829358362135124927, 7.499999999999999112, -14.27056707468146435 ) ) ;
#17363 = CARTESIAN_POINT ( 'NONE',  ( 0.3058872367615226295, 13.24582953854930345, -3.664492643742625511 ) ) ;
#17364 = CARTESIAN_POINT ( 'NONE',  ( 0.3142011359265332593, -10.88514493056448096, 8.382042760265870029 ) ) ;
#17365 = AXIS2_PLACEMENT_3D ( 'NONE', #18626, #14519, #4086 ) ;
#17366 = CARTESIAN_POINT ( 'NONE',  ( 2.002547531651519996, -7.942910686618100513, -9.778737580845787036 ) ) ;
#17367 = CARTESIAN_POINT ( 'NONE',  ( 1.847412631396506244, 3.804043368582664009, 11.84727953344284579 ) ) ;
#17368 = CARTESIAN_POINT ( 'NONE',  ( 0.3137051932979792457, 4.679953077377485116, 12.91601973349272114 ) ) ;
#17369 = B_SPLINE_CURVE_WITH_KNOTS ( 'NONE', 3,
 ( #10704, #3526, #12317, #9361 ),
 .UNSPECIFIED., .F., .F.,
 ( 4, 4 ),
 ( 0.000000000000000000, 0.002004993803841771411 ),
 .UNSPECIFIED. ) ;
#17370 = CARTESIAN_POINT ( 'NONE',  ( 1.560000000000000053, -0.8660254037844384856, 1.500000000000000000 ) ) ;
#17371 = VECTOR ( 'NONE', #4758, 1000.000000000000000 ) ;
#17372 = VERTEX_POINT ( 'NONE', #10514 ) ;
#17373 = ORIENTED_EDGE ( 'NONE', *, *, #15576, .F. ) ;
#17374 = ORIENTED_EDGE ( 'NONE', *, *, #5244, .F. ) ;
#17375 = AXIS2_PLACEMENT_3D ( 'NONE', #4006, #2554, #8405 ) ;
#17376 = ORIENTED_EDGE ( 'NONE', *, *, #12072, .F. ) ;
#17377 = CARTESIAN_POINT ( 'NONE',  ( 1.560000000000000053, 1.732050807568878747, 7.017607234860990640E-28 ) ) ;
#17378 = ADVANCED_FACE ( 'NONE', ( #10617 ), #12195, .F. ) ;
#17379 = ORIENTED_EDGE ( 'NONE', *, *, #6121, .F. ) ;
#17380 = DIRECTION ( 'NONE',  ( -1.000000000000000000, 0.000000000000000000, 0.000000000000000000 ) ) ;
#17381 = CARTESIAN_POINT ( 'NONE',  ( -105.8941953964643261, -81.60345299795268659, -89.13679372318456728 ) ) ;
#17382 = DIRECTION ( 'NONE',  ( 0.000000000000000000, 0.000000000000000000, -1.000000000000000000 ) ) ;
#17383 = FACE_OUTER_BOUND ( 'NONE', #17550, .T. ) ;
#17384 = ORIENTED_EDGE ( 'NONE', *, *, #5419, .T. ) ;
#17385 = CARTESIAN_POINT ( 'NONE',  ( -199.9999999999999716, 9.999999999999973355, 6.000000000000000000 ) ) ;
#17386 = ADVANCED_FACE ( 'NONE', ( #6021 ), #1282, .F. ) ;
#17387 = DIRECTION ( 'NONE',  ( 0.000000000000000000, 1.224646799147353207E-16, -1.000000000000000000 ) ) ;
#17388 = CARTESIAN_POINT ( 'NONE',  ( 0.4862570985993252548, 12.97920246947879441, 5.003653737315533867 ) ) ;
#17389 = CARTESIAN_POINT ( 'NONE',  ( 0.3142011359265306503, -13.17934269988455576, -3.879426116491829557 ) ) ;
#17390 = CARTESIAN_POINT ( 'NONE',  ( 2.636624412714236865, 0.000000000000000000, 0.000000000000000000 ) ) ;
#17391 = CARTESIAN_POINT ( 'NONE',  ( 0.000000000000000000, 0.000000000000000000, 0.000000000000000000 ) ) ;
#17392 = CARTESIAN_POINT ( 'NONE',  ( -199.9999999999999716, 9.999999999999973355, 6.000000000000000000 ) ) ;
#17393 = ORIENTED_EDGE ( 'NONE', *, *, #6525, .T. ) ;
#17394 = CARTESIAN_POINT ( 'NONE',  ( 1.847372867223025183, 7.398914411685134418, -10.00438561114516034 ) ) ;
#17396 = EDGE_LOOP ( 'NONE', ( #6751, #16236, #6017, #17210 ) ) ;
#17395 = DIRECTION ( 'NONE',  ( -0.000000000000000000, 0.000000000000000000, -1.000000000000000000 ) ) ;
#17397 = CARTESIAN_POINT ( 'NONE',  ( 0.3151928476913555821, 8.075547435847115096, -11.11539186930577827 ) ) ;
#17398 = ORIENTED_EDGE ( 'NONE', *, *, #14979, .T. ) ;
#17399 = CARTESIAN_POINT ( 'NONE',  ( 0.3170788640506440603, -13.11595226728160668, 4.100430649997911736 ) ) ;
#17400 = ORIENTED_EDGE ( 'NONE', *, *, #8833, .F. ) ;
#17401 = CARTESIAN_POINT ( 'NONE',  ( 1.847380140988739594, 10.13114603776196887, 7.224522571381366554 ) ) ;
#17402 = B_SPLINE_CURVE_WITH_KNOTS ( 'NONE', 3,
 ( #4125, #15677, #4227, #111 ),
 .UNSPECIFIED., .F., .F.,
 ( 4, 4 ),
 ( 1.514782153580211930E-17, 0.003005512676784846161 ),
 .UNSPECIFIED. ) ;
#17403 = CARTESIAN_POINT ( 'NONE',  ( 5.641944871949947427, -4.153144983956821079, -12.00000000256098254 ) ) ;
#17404 = B_SPLINE_CURVE_WITH_KNOTS ( 'NONE', 3,
 ( #3188, #11906, #16410, #9038, #10277, #10177 ),
 .UNSPECIFIED., .F., .F.,
 ( 4, 2, 4 ),
 ( 4.256846838097967453E-17, 0.0002014099069817298958, 0.0004028198139634172367 ),
 .UNSPECIFIED. ) ;
#17405 = ORIENTED_EDGE ( 'NONE', *, *, #2048, .F. ) ;
#17406 = VECTOR ( 'NONE', #5619, 1000.000000000000000 ) ;
#17407 = CARTESIAN_POINT ( 'NONE',  ( 0.3095370825347224519, -4.681152801286251552, 12.91933430393606486 ) ) ;
#17408 = ADVANCED_FACE ( 'NONE', ( #9172 ), #4389, .T. ) ;
#17409 = ADVANCED_FACE ( 'NONE', ( #13181 ), #1923, .T. ) ;
#17410 = EDGE_CURVE ( 'NONE', #16292, #17234, #1023, .T. ) ;
#17411 = CARTESIAN_POINT ( 'NONE',  ( -4.999999999999995559, -30.00000000000000000, 31.00000000000000000 ) ) ;
#17412 = CARTESIAN_POINT ( 'NONE',  ( 1.846524061778019199, -9.853584647934329865, -7.597197846158187495 ) ) ;
#17413 = CARTESIAN_POINT ( 'NONE',  ( 2.320520222536399668, 3.126729907239529815, 15.43440824796666710 ) ) ;
#17414 = EDGE_LOOP ( 'NONE', ( #13166, #11489, #4365, #2737 ) ) ;
#17415 = B_SPLINE_CURVE_WITH_KNOTS ( 'NONE', 3,
 ( #7588, #13584, #4608, #10726, #4984, #9191 ),
 .UNSPECIFIED., .F., .F.,
 ( 4, 2, 4 ),
 ( 4.027530160694267299E-17, 0.0002014099069817290827, 0.0004028198139634178872 ),
 .UNSPECIFIED. ) ;
#17416 = B_SPLINE_CURVE_WITH_KNOTS ( 'NONE', 3,
 ( #18689, #5592, #17263, #4183, #7825, #1983 ),
 .UNSPECIFIED., .F., .F.,
 ( 4, 2, 4 ),
 ( 0.000000000000000000, 0.001500839035891553090, 0.003001678071783106180 ),
 .UNSPECIFIED. ) ;
#17417 = FILL_AREA_STYLE_COLOUR ( '', #6622 ) ;
#17418 = FACE_OUTER_BOUND ( 'NONE', #4555, .T. ) ;
#17419 = CARTESIAN_POINT ( 'NONE',  ( 2.123976203522053297, 10.37815841598508371, -11.67822624909914175 ) ) ;
#17420 = CARTESIAN_POINT ( 'NONE',  ( 0.3095370825347233956, -4.681152801286073917, -12.91933430393612525 ) ) ;
#17421 = CARTESIAN_POINT ( 'NONE',  ( 2.747332970342022840, 11.66639548242807578, 11.45495994260722306 ) ) ;
#17422 = CARTESIAN_POINT ( 'NONE',  ( 2.636624412714236865, 15.91454522070173638, 2.161493821596668585 ) ) ;
#17423 = APPLICATION_CONTEXT ( 'automotive_design' ) ;
#17424 = ORIENTED_EDGE ( 'NONE', *, *, #13287, .T. ) ;
#17425 = CARTESIAN_POINT ( 'NONE',  ( 16.56753206892534891, 0.006760771273035115839, -0.006669401563385219701 ) ) ;
#17426 = CARTESIAN_POINT ( 'NONE',  ( 16.56753206892534891, -0.006760771273036217388, -0.006669401563384900512 ) ) ;
#17427 = B_SPLINE_CURVE_WITH_KNOTS ( 'NONE', 3,
 ( #11923, #4664, #10492, #3207, #1797, #12391 ),
 .UNSPECIFIED., .F., .F.,
 ( 4, 2, 4 ),
 ( 3.361796080452501619E-17, 0.0001825746017570592115, 0.0003651492035140848128 ),
 .UNSPECIFIED. ) ;
#17428 = ORIENTED_EDGE ( 'NONE', *, *, #18267, .F. ) ;
#17429 = ORIENTED_EDGE ( 'NONE', *, *, #5186, .T. ) ;
#17431 = CARTESIAN_POINT ( 'NONE',  ( 1.342453679581834924, -14.76648944001038544, -0.9602753779832271519 ) ) ;
#17430 = CIRCLE ( 'NONE', #4308, 16.06066017081991149 ) ;
#17432 = ORIENTED_EDGE ( 'NONE', *, *, #18238, .F. ) ;
#17433 = CARTESIAN_POINT ( 'NONE',  ( 2.636624412715137922, -7.605649742761668719, 14.14563173255331741 ) ) ;
#17434 = ORIENTED_EDGE ( 'NONE', *, *, #8575, .F. ) ;
#17435 = EDGE_CURVE ( 'NONE', #14697, #4455, #17172, .T. ) ;
#17436 = ADVANCED_FACE ( 'NONE', ( #16127 ), #12789, .T. ) ;
#17437 = ADVANCED_FACE ( 'NONE', ( #16325 ), #67, .F. ) ;
#17438 = CARTESIAN_POINT ( 'NONE',  ( 0.3939875929385642239, 13.34133634968955917, 3.598491969338272867 ) ) ;
#17439 = ADVANCED_FACE ( 'NONE', ( #2912 ), #11828, .T. ) ;
#17440 = CARTESIAN_POINT ( 'NONE',  ( 1.254255976358046087, 5.487601330835574664, -13.61551404021248857 ) ) ;
#17441 = PRODUCT_DEFINITION_SHAPE ( 'NONE', 'NONE',  #18914 ) ;
#17442 = CARTESIAN_POINT ( 'NONE',  ( 0.3148213771069373057, -8.260246460850796169, 10.97836617636221845 ) ) ;
#17443 = CARTESIAN_POINT ( 'NONE',  ( 2.002547531651519996, -4.532360870844247991, -11.75462648437106417 ) ) ;
#17444 = CARTESIAN_POINT ( 'NONE',  ( 0.000000000000000000, 0.000000000000000000, 0.000000000000000000 ) ) ;
#17445 = AXIS2_PLACEMENT_3D ( 'NONE', #5726, #10421, #12904 ) ;
#17446 = CARTESIAN_POINT ( 'NONE',  ( 1.959283090834842200, 4.509128209890970851, 11.71721539537256618 ) ) ;
#17447 = CARTESIAN_POINT ( 'NONE',  ( 16.57210152137263393, 0.005118120558001383255, -0.01361613799508856922 ) ) ;
#17448 = CARTESIAN_POINT ( 'NONE',  ( 0.3150686449036029790, 13.73846184595214304, -0.1533607327086227434 ) ) ;
#17449 = VERTEX_POINT ( 'NONE', #8951 ) ;
#17450 = ORIENTED_EDGE ( 'NONE', *, *, #5857, .F. ) ;
#17451 = ORIENTED_EDGE ( 'NONE', *, *, #17186, .F. ) ;
#17452 = B_SPLINE_CURVE_WITH_KNOTS ( 'NONE', 3,
 ( #12503, #11086, #11177, #14035 ),
 .UNSPECIFIED., .F., .F.,
 ( 4, 4 ),
 ( 0.000000000000000000, 0.002004993803842297466 ),
 .UNSPECIFIED. ) ;
#17453 = ORIENTED_EDGE ( 'NONE', *, *, #11050, .T. ) ;
#17454 = ORIENTED_EDGE ( 'NONE', *, *, #4634, .F. ) ;
#17455 = CARTESIAN_POINT ( 'NONE',  ( 1.847034903785822246, 4.063013886994871982, -11.76058231742741533 ) ) ;
#17456 = CARTESIAN_POINT ( 'NONE',  ( 2.002547531651519996, -0.6781519942170860515, -12.57989064830760206 ) ) ;
#17457 = CARTESIAN_POINT ( 'NONE',  ( 0.3142011359265349801, 7.762194356530932815, -11.33549115679415031 ) ) ;
#17458 = VERTEX_POINT ( 'NONE', #265 ) ;
#17459 = CYLINDRICAL_SURFACE ( 'NONE', #8098, 1.000000000000000000 ) ;
#17460 = DIRECTION ( 'NONE',  ( 0.000000000000000000, 0.000000000000000000, 1.000000000000000000 ) ) ;
#17461 = EDGE_CURVE ( 'NONE', #5518, #15560, #1866, .T. ) ;
#17462 = CARTESIAN_POINT ( 'NONE',  ( 0.3095370825347234511, 0.4597470195092124290, -13.73357284481724250 ) ) ;
#17463 = DIRECTION ( 'NONE',  ( 0.000000000000000000, 0.000000000000000000, 1.000000000000000000 ) ) ;
#17464 = CARTESIAN_POINT ( 'NONE',  ( 0.4754618798421162973, 3.583352865732667425, 13.45049478164061441 ) ) ;
#17465 = VECTOR ( 'NONE', #5925, 1000.000000000000114 ) ;
#17466 = B_SPLINE_CURVE_WITH_KNOTS ( 'NONE', 3,
 ( #9343, #9436, #11059, #18310, #16606, #3504 ),
 .UNSPECIFIED., .F., .F.,
 ( 4, 2, 4 ),
 ( 0.000000000000000000, 0.0001828790815886945087, 0.0003657581631773890174 ),
 .UNSPECIFIED. ) ;
#17467 = CARTESIAN_POINT ( 'NONE',  ( 2.747332970342022840, -16.17136872824900351, 2.409922051470623661 ) ) ;
#17468 = CARTESIAN_POINT ( 'NONE',  ( 1.918921323896323639, -9.738309537478938793, -7.860085869556288962 ) ) ;
#17469 = DIRECTION ( 'NONE',  ( 0.000000000000000000, 0.000000000000000000, 1.000000000000000000 ) ) ;
#17470 = CARTESIAN_POINT ( 'NONE',  ( 0.3142011359265305392, 3.879426116491875742, -13.17934269988453977 ) ) ;
#17471 = VERTEX_POINT ( 'NONE', #10588 ) ;
#17472 = ORIENTED_EDGE ( 'NONE', *, *, #14053, .F. ) ;
#17473 = ORIENTED_EDGE ( 'NONE', *, *, #6828, .F. ) ;
#17474 = EDGE_CURVE ( 'NONE', #15726, #5898, #11633, .T. ) ;
#17475 = ORIENTED_EDGE ( 'NONE', *, *, #11302, .T. ) ;
#17476 = VERTEX_POINT ( 'NONE', #6095 ) ;
#17477 = FACE_OUTER_BOUND ( 'NONE', #3495, .T. ) ;
#17478 = CARTESIAN_POINT ( 'NONE',  ( 3.950837973638676281, -10.05648675950133963, 10.51028938476214059 ) ) ;
#17479 = DIRECTION ( 'NONE',  ( -1.000000000000000000, -0.000000000000000000, -0.000000000000000000 ) ) ;
#17480 = CARTESIAN_POINT ( 'NONE',  ( -194.9999999999999716, -10.00000000000002665, 3.000000000000002665 ) ) ;
#17481 = ORIENTED_EDGE ( 'NONE', *, *, #16626, .T. ) ;
#17482 = CARTESIAN_POINT ( 'NONE',  ( 1.918921323896324971, 0.6349083173281891979, -12.49850046818173688 ) ) ;
#17483 = CARTESIAN_POINT ( 'NONE',  ( 0.3150686449036048664, -4.391272911157235725, -13.01866258978841628 ) ) ;
#17484 = CARTESIAN_POINT ( 'NONE',  ( 1.342453679581834924, 0.9602753779830727199, 14.76648944001039787 ) ) ;
#17485 = DIRECTION ( 'NONE',  ( 0.000000000000000000, 0.000000000000000000, 1.000000000000000000 ) ) ;
#17486 = CARTESIAN_POINT ( 'NONE',  ( 1.846613052777652975, 11.93415846513961753, 3.520031056876344433 ) ) ;
#17487 = CARTESIAN_POINT ( 'NONE',  ( 2.353870697619111496, -12.92712089195302561, -0.7635393531607687079 ) ) ;
#17488 = CARTESIAN_POINT ( 'NONE',  ( 16.56679352167444819, -0.001390132774594504727, 0.009190982326619714232 ) ) ;
#17489 = ORIENTED_EDGE ( 'NONE', *, *, #10814, .T. ) ;
#17490 = DIRECTION ( 'NONE',  ( -1.000000000000000000, -0.000000000000000000, -0.000000000000000000 ) ) ;
#17492 = ORIENTED_EDGE ( 'NONE', *, *, #1160, .F. ) ;
#17491 = DIRECTION ( 'NONE',  ( -1.000000000000000000, 0.000000000000000000, 0.000000000000000000 ) ) ;
#17493 = CARTESIAN_POINT ( 'NONE',  ( 16.56782317627811096, -0.007739510688078479403, 0.006045301465876602373 ) ) ;
#17494 = B_SPLINE_CURVE_WITH_KNOTS ( 'NONE', 3,
 ( #15196, #3714, #11269, #13935, #12588, #10903 ),
 .UNSPECIFIED., .F., .F.,
 ( 4, 2, 4 ),
 ( 0.000000000000000000, 0.001656992708822040920, 0.003313985417644081839 ),
 .UNSPECIFIED. ) ;
#17495 = AXIS2_PLACEMENT_3D ( 'NONE', #2777, #7394, #17510 ) ;
#17496 = EDGE_CURVE ( 'NONE', #256, #5504, #4568, .T. ) ;
#17497 = CARTESIAN_POINT ( 'NONE',  ( 0.000000000000000000, 5.817072295949927426E-16, -4.750000000000000000 ) ) ;
#17498 =( BOUNDED_SURFACE ( )  B_SPLINE_SURFACE ( 3, 1, ( 
 ( #11409, #4141 ),
 ( #16954, #9856 ),
 ( #15513, #8267 ),
 ( #901, #3765 ) ),
 .UNSPECIFIED., .F., .F., .T. ) 
 B_SPLINE_SURFACE_WITH_KNOTS ( ( 4, 4 ),
 ( 2, 2 ),
 ( 0.000000000000000000, 1.000000000000000000 ),
 ( 0.000000000000000000, 1.000000000000000000 ),
 .UNSPECIFIED. ) 
 GEOMETRIC_REPRESENTATION_ITEM ( )  RATIONAL_B_SPLINE_SURFACE ( (
 ( 1.000000000000000000, 1.000000000000000000),
 ( 0.9933953342250436691, 0.8357391271907733676),
 ( 0.9933953342250436691, 0.8357391271907733676),
 ( 1.000000000000000000, 1.000000000000000000) ) ) 
 REPRESENTATION_ITEM ( '' )  SURFACE ( )  );
#17499 = VERTEX_POINT ( 'NONE', #17758 ) ;
#17500 = EDGE_CURVE ( 'NONE', #1614, #5120, #15249, .T. ) ;
#17501 = CARTESIAN_POINT ( 'NONE',  ( 0.3151930723728413319, 4.318364831037771800, -13.04315954105010533 ) ) ;
#17502 = FACE_OUTER_BOUND ( 'NONE', #14001, .T. ) ;
#17503 = ORIENTED_EDGE ( 'NONE', *, *, #5487, .F. ) ;
#17504 = CARTESIAN_POINT ( 'NONE',  ( 16.56753206892534891, -0.008490833999798956880, -0.004253784598196145433 ) ) ;
#17505 = CARTESIAN_POINT ( 'NONE',  ( 1.846138399168762101, 3.446241763653166590, -11.95493567637846866 ) ) ;
#17506 = CARTESIAN_POINT ( 'NONE',  ( 3.686287386450715076E-15, -16.60000000000000142, 21.01316734529526187 ) ) ;
#17507 = DIRECTION ( 'NONE',  ( 0.000000000000000000, 0.000000000000000000, -1.000000000000000000 ) ) ;
#17508 = AXIS2_PLACEMENT_3D ( 'NONE', #2689, #17226, #17323 ) ;
#17509 = AXIS2_PLACEMENT_3D ( 'NONE', #4296, #2658, #2834 ) ;
#17510 = DIRECTION ( 'NONE',  ( 0.000000000000000000, 0.5000000000000003331, -0.8660254037844383745 ) ) ;
#17511 = CARTESIAN_POINT ( 'NONE',  ( 0.3307726912345181902, 10.76786801061219734, -8.558645027434160113 ) ) ;
#17512 = DIRECTION ( 'NONE',  ( 0.000000000000000000, 0.000000000000000000, -1.000000000000000000 ) ) ;
#17513 = DIRECTION ( 'NONE',  ( 0.000000000000000000, 0.000000000000000000, 1.000000000000000000 ) ) ;
#17514 = CARTESIAN_POINT ( 'NONE',  ( 2.002547531651519996, -6.845637710436110801, -10.57595306287299763 ) ) ;
#17515 = ADVANCED_FACE ( 'NONE', ( #16425 ), #16199, .F. ) ;
#17516 = ORIENTED_EDGE ( 'NONE', *, *, #13472, .T. ) ;
#17517 = CARTESIAN_POINT ( 'NONE',  ( 0.3142014840576516921, 11.33546131209473806, -7.762239086932731347 ) ) ;
#17518 = CARTESIAN_POINT ( 'NONE',  ( 16.56679352167444819, 0.009190982326619362083, -0.001390132774595485713 ) ) ;
#17519 = ORIENTED_EDGE ( 'NONE', *, *, #4635, .F. ) ;
#17520 = ORIENTED_EDGE ( 'NONE', *, *, #7685, .F. ) ;
#17521 = CARTESIAN_POINT ( 'NONE',  ( 0.3132635586635976188, -4.743936529203153007, -12.89236642382226172 ) ) ;
#17522 = ORIENTED_EDGE ( 'NONE', *, *, #10868, .F. ) ;
#17523 = CYLINDRICAL_SURFACE ( 'NONE', #14713, 5.000000000000004441 ) ;
#17524 = B_SPLINE_CURVE_WITH_KNOTS ( 'NONE', 3,
 ( #5965, #1667, #7227, #243, #13040, #14662 ),
 .UNSPECIFIED., .F., .F.,
 ( 4, 2, 4 ),
 ( 0.000000000000000000, 0.001656992708824380845, 0.003313985417648761689 ),
 .UNSPECIFIED. ) ;
#17525 = EDGE_LOOP ( 'NONE', ( #2265, #12675, #18078, #6805 ) ) ;
#17526 = FACE_OUTER_BOUND ( 'NONE', #13676, .T. ) ;
#17527 = CARTESIAN_POINT ( 'NONE',  ( 16.58200780006414732, 0.01115192838421469497, -0.0006320991582341122352 ) ) ;
#17528 = CARTESIAN_POINT ( 'NONE',  ( 3.950837973638668288, 0.000000000000000000, 0.000000000000000000 ) ) ;
#17529 = CARTESIAN_POINT ( 'NONE',  ( 0.3939822652208126996, -8.678192463540247203, 10.75310269629518700 ) ) ;
#17530 = B_SPLINE_CURVE_WITH_KNOTS ( 'NONE', 3,
 ( #7597, #13118, #10444, #3163, #9011, #25 ),
 .UNSPECIFIED., .F., .F.,
 ( 4, 2, 4 ),
 ( 2.474737474518078493E-18, 0.0002017457492448081235, 0.0004034914984896138075 ),
 .UNSPECIFIED. ) ;
#17531 = FACE_OUTER_BOUND ( 'NONE', #5728, .T. ) ;
#17533 = FACE_OUTER_BOUND ( 'NONE', #8424, .T. ) ;
#17532 =( BOUNDED_SURFACE ( )  B_SPLINE_SURFACE ( 3, 1, ( 
 ( #14740, #5847 ),
 ( #17518, #4425 ),
 ( #10259, #14648 ),
 ( #13212, #127 ) ),
 .UNSPECIFIED., .F., .F., .T. ) 
 B_SPLINE_SURFACE_WITH_KNOTS ( ( 4, 4 ),
 ( 2, 2 ),
 ( 0.000000000000000000, 1.000000000000000000 ),
 ( 0.000000000000000000, 1.000000000000000000 ),
 .UNSPECIFIED. ) 
 GEOMETRIC_REPRESENTATION_ITEM ( )  RATIONAL_B_SPLINE_SURFACE ( (
 ( 1.000000000000000000, 1.000000000000000000),
 ( 0.9593108457356467333, 0.9995965569486454649),
 ( 0.9593108457356467333, 0.9995965569486454649),
 ( 1.000000000000000000, 1.000000000000000000) ) ) 
 REPRESENTATION_ITEM ( '' )  SURFACE ( )  );
#17534 =( BOUNDED_SURFACE ( )  B_SPLINE_SURFACE ( 3, 1, ( 
 ( #4346, #5764 ),
 ( #6940, #11609 ),
 ( #10171, #11245 ),
 ( #11333, #17150 ) ),
 .UNSPECIFIED., .F., .F., .T. ) 
 B_SPLINE_SURFACE_WITH_KNOTS ( ( 4, 4 ),
 ( 2, 2 ),
 ( 0.000000000000000000, 1.000000000000000000 ),
 ( 0.000000000000000000, 1.000000000000000000 ),
 .UNSPECIFIED. ) 
 GEOMETRIC_REPRESENTATION_ITEM ( )  RATIONAL_B_SPLINE_SURFACE ( (
 ( 1.000000000000000000, 1.000000000000000000),
 ( 0.9933953342250436691, 0.8357391271907733676),
 ( 0.9933953342250436691, 0.8357391271907733676),
 ( 1.000000000000000000, 1.000000000000000000) ) ) 
 REPRESENTATION_ITEM ( '' )  SURFACE ( )  );
#17535 = AXIS2_PLACEMENT_3D ( 'NONE', #11752, #7270, #13083 ) ;
#17536 =( NAMED_UNIT ( * ) SI_UNIT ( $, .STERADIAN. ) SOLID_ANGLE_UNIT ( ) );
#17537 = CARTESIAN_POINT ( 'NONE',  ( 2.747332970342022840, -11.45495994260726214, 11.66639548242803492 ) ) ;
#17538 = DIRECTION ( 'NONE',  ( 0.000000000000000000, -0.000000000000000000, -1.000000000000000000 ) ) ;
#17539 = FACE_OUTER_BOUND ( 'NONE', #7504, .T. ) ;
#17540 = AXIS2_PLACEMENT_3D ( 'NONE', #7654, #4771, #6492 ) ;
#17541 = CARTESIAN_POINT ( 'NONE',  ( 0.3145729642390356351, 13.73540280162741034, -0.3065092323351694126 ) ) ;
#17542 = EDGE_CURVE ( 'NONE', #13455, #6415, #5173, .T. ) ;
#17543 = ORIENTED_EDGE ( 'NONE', *, *, #2290, .F. ) ;
#17544 = EDGE_CURVE ( 'NONE', #3029, #8074, #6306, .T. ) ;
#17545 = AXIS2_PLACEMENT_3D ( 'NONE', #2007, #9069, #1906 ) ;
#17546 = CARTESIAN_POINT ( 'NONE',  ( -61.35602477868047799, -10.00000000000000888, 6.000000000000000000 ) ) ;
#17547 = ORIENTED_EDGE ( 'NONE', *, *, #14599, .F. ) ;
#17548 = VERTEX_POINT ( 'NONE', #17665 ) ;
#17549 = ORIENTED_EDGE ( 'NONE', *, *, #2756, .T. ) ;
#17550 = EDGE_LOOP ( 'NONE', ( #6003, #4897, #16846, #6975 ) ) ;
#17551 = DIRECTION ( 'NONE',  ( -1.000000000000000000, 0.000000000000000000, 0.000000000000000000 ) ) ;
#17552 = AXIS2_PLACEMENT_3D ( 'NONE', #3668, #5008, #11128 ) ;
#17553 = CARTESIAN_POINT ( 'NONE',  ( 3.512766787570801519, 6.535475144496956545, 13.55823433651946175 ) ) ;
#17554 = VECTOR ( 'NONE', #17062, 1000.000000000000114 ) ;
#17555 = LINE ( 'NONE', #18599, #2028 ) ;
#17556 = ORIENTED_EDGE ( 'NONE', *, *, #10097, .F. ) ;
#17557 = DIRECTION ( 'NONE',  ( -0.7071067811865474617, 0.000000000000000000, 0.7071067811865474617 ) ) ;
#17558 = CARTESIAN_POINT ( 'NONE',  ( 1.846138399168762101, -11.95493567637852905, 3.446241763652952539 ) ) ;
#17559 = CARTESIAN_POINT ( 'NONE',  ( 0.8740764193768836288, 9.070946295054209685, -11.05257066464527327 ) ) ;
#17560 = CARTESIAN_POINT ( 'NONE',  ( 2.705023505549867924, -0.8488853074252048492, -13.27418276223637150 ) ) ;
#17561 = FACE_OUTER_BOUND ( 'NONE', #17007, .T. ) ;
#17562 = CARTESIAN_POINT ( 'NONE',  ( 1.846822687350021974, 0.2922081769261886675, -12.43915556955403190 ) ) ;
#17563 = CARTESIAN_POINT ( 'NONE',  ( 0.4862570985993235340, 8.769551628660735787, 10.79774104611376373 ) ) ;
#17564 = FACE_OUTER_BOUND ( 'NONE', #6033, .T. ) ;
#17565 = CARTESIAN_POINT ( 'NONE',  ( 0.3148213771069321987, -7.888490156175138601, -11.24846294176320960 ) ) ;
#17566 = EDGE_LOOP ( 'NONE', ( #14703, #18573, #8889, #17920, #3889, #5982, #15565, #6916, #12267, #7791, #14480, #9398 ) ) ;
#17567 = AXIS2_PLACEMENT_3D ( 'NONE', #6820, #6647, #12639 ) ;
#17568 = VERTEX_POINT ( 'NONE', #18888 ) ;
#17569 = ORIENTED_EDGE ( 'NONE', *, *, #17611, .F. ) ;
#17570 = EDGE_CURVE ( 'NONE', #3103, #7378, #16021, .T. ) ;
#17571 = ORIENTED_EDGE ( 'NONE', *, *, #3323, .T. ) ;
#17572 = CARTESIAN_POINT ( 'NONE',  ( 0.3095370825347233956, -3.806662003783505277, 13.20347358821913275 ) ) ;
#17573 = EDGE_CURVE ( 'NONE', #16490, #5397, #14588, .T. ) ;
#17574 = ORIENTED_EDGE ( 'NONE', *, *, #272, .F. ) ;
#17575 = DIRECTION ( 'NONE',  ( -1.000000000000000000, -0.000000000000000000, -0.000000000000000000 ) ) ;
#17576 = CARTESIAN_POINT ( 'NONE',  ( 0.8740764193767813772, -12.04241474977994208, 7.708542792189371440 ) ) ;
#17577 = DIRECTION ( 'NONE',  ( 1.182917971378669595E-16, 0.2588190451025206285, -0.9659258262890683122 ) ) ;
#17578 = CARTESIAN_POINT ( 'NONE',  ( 1.861706995891670546, -12.00328602385077659, -3.332865258614104320 ) ) ;
#17579 = ORIENTED_EDGE ( 'NONE', *, *, #9378, .F. ) ;
#17580 = CARTESIAN_POINT ( 'NONE',  ( 2.949999999999999734, 3.306546357697853240E-16, -2.699999999999999734 ) ) ;
#17581 = ADVANCED_FACE ( 'NONE', ( #1505 ), #3106, .F. ) ;
#17582 = CARTESIAN_POINT ( 'NONE',  ( 2.002547531651519996, 10.57595306287302250, -6.845637710436074386 ) ) ;
#17583 = CONICAL_SURFACE ( 'NONE', #11485, 14.54644660717763927, 0.8559913436420816257 ) ;
#17584 = CARTESIAN_POINT ( 'NONE',  ( 16.57210152137263393, 0.01402404281922921964, -0.003862718596009325888 ) ) ;
#17585 = B_SPLINE_CURVE_WITH_KNOTS ( 'NONE', 3,
 ( #812, #6551, #10760, #9320, #15050, #4926 ),
 .UNSPECIFIED., .F., .F.,
 ( 4, 2, 4 ),
 ( 3.556447555475521540E-17, 0.0001825746017570587236, 0.0003651492035140818855 ),
 .UNSPECIFIED. ) ;
#17586 = CIRCLE ( 'NONE', #15151, 2.750000000000000000 ) ;
#17587 = CARTESIAN_POINT ( 'NONE',  ( 3.950837973638677170, 10.51028938476232355, -10.05648675950114956 ) ) ;
#17588 = SURFACE_SIDE_STYLE ('',( #13566 ) ) ;
#17589 = FACE_OUTER_BOUND ( 'NONE', #14595, .T. ) ;
#17590 = VERTEX_POINT ( 'NONE', #1987 ) ;
#17591 = EDGE_CURVE ( 'NONE', #7061, #13310, #17466, .T. ) ;
#17592 = CARTESIAN_POINT ( 'NONE',  ( 1.846524061778019199, 7.597197846158221246, -9.853584647934303220 ) ) ;
#17594 = ORIENTED_EDGE ( 'NONE', *, *, #926, .F. ) ;
#17593 = CARTESIAN_POINT ( 'NONE',  ( 1.321128355694181398E-14, -7.013167318348350499, 25.01316734529530095 ) ) ;
#17595 = DIRECTION ( 'NONE',  ( 1.000000000000000000, 0.000000000000000000, 0.000000000000000000 ) ) ;
#17596 = EDGE_CURVE ( 'NONE', #2807, #10634, #12120, .T. ) ;
#17597 = EDGE_CURVE ( 'NONE', #10307, #1375, #18148, .T. ) ;
#17598 = DIRECTION ( 'NONE',  ( 2.891205793294679312E-16, -1.000000000000000000, -0.000000000000000000 ) ) ;
#17599 = ORIENTED_EDGE ( 'NONE', *, *, #9512, .T. ) ;
#17600 = CARTESIAN_POINT ( 'NONE',  ( 3.950837973638675393, -10.51028938476210328, -10.05648675950137871 ) ) ;
#17601 = UNCERTAINTY_MEASURE_WITH_UNIT (LENGTH_MEASURE( 1.000000000000000082E-05 ), #13891, 'distance_accuracy_value', 'NONE');
#17602 = B_SPLINE_CURVE_WITH_KNOTS ( 'NONE', 3,
 ( #247, #11525, #12374, #9417, #13621, #2157 ),
 .UNSPECIFIED., .F., .F.,
 ( 4, 2, 4 ),
 ( 3.551420023959826846E-17, 0.0001825746017570578021, 0.0003651492035140800965 ),
 .UNSPECIFIED. ) ;
#17603 = DIRECTION ( 'NONE',  ( 1.224646799147353207E-16, 1.000000000000000000, -0.000000000000000000 ) ) ;
#17604 = ORIENTED_EDGE ( 'NONE', *, *, #18161, .T. ) ;
#17605 = DIRECTION ( 'NONE',  ( -0.000000000000000000, -0.000000000000000000, 1.000000000000000000 ) ) ;
#17606 = CARTESIAN_POINT ( 'NONE',  ( 16.58200780006414732, 0.004047297414159048250, -0.01041078477704050417 ) ) ;
#17607 = CIRCLE ( 'NONE', #18221, 14.54644660717763927 ) ;
#17608 = CARTESIAN_POINT ( 'NONE',  ( 0.3132635586635980074, -10.79541209008109703, 8.495712071659360376 ) ) ;
#17609 = CARTESIAN_POINT ( 'NONE',  ( 0.3939875929385656117, -13.80036004410495210, 0.7003304234512695015 ) ) ;
#17610 = AXIS2_PLACEMENT_3D ( 'NONE', #836, #10886, #2356 ) ;
#17611 = EDGE_CURVE ( 'NONE', #13213, #4341, #9711, .T. ) ;
#17612 = VECTOR ( 'NONE', #1571, 1000.000000000000114 ) ;
#17614 = VECTOR ( 'NONE', #18538, 1000.000000000000114 ) ;
#17613 = CARTESIAN_POINT ( 'NONE',  ( 16.56822296793089322, -0.005339139727952723832, 0.008619100080559757848 ) ) ;
#17615 = B_SPLINE_CURVE_WITH_KNOTS ( 'NONE', 3,
 ( #4244, #16087, #13119, #18853, #7398, #5745 ),
 .UNSPECIFIED., .F., .F.,
 ( 4, 2, 4 ),
 ( 2.168404344971008868E-19, 0.0001828790815886944003, 0.0003657581631773885837 ),
 .UNSPECIFIED. ) ;
#17616 =( BOUNDED_SURFACE ( )  B_SPLINE_SURFACE ( 3, 1, ( 
 ( #13044, #8931 ),
 ( #7519, #1579 ),
 ( #16305, #5971 ),
 ( #14760, #17834 ) ),
 .UNSPECIFIED., .F., .F., .T. ) 
 B_SPLINE_SURFACE_WITH_KNOTS ( ( 4, 4 ),
 ( 2, 2 ),
 ( 0.000000000000000000, 1.000000000000000000 ),
 ( 0.000000000000000000, 1.000000000000000000 ),
 .UNSPECIFIED. ) 
 GEOMETRIC_REPRESENTATION_ITEM ( )  RATIONAL_B_SPLINE_SURFACE ( (
 ( 1.000000000000000000, 1.000000000000000000),
 ( 0.9593108457356467333, 0.9995965569486454649),
 ( 0.9593108457356467333, 0.9995965569486454649),
 ( 1.000000000000000000, 1.000000000000000000) ) ) 
 REPRESENTATION_ITEM ( '' )  SURFACE ( )  );
#17617 = CARTESIAN_POINT ( 'NONE',  ( 16.56872352241294521, -0.007512283835804365630, 0.007240717549633862542 ) ) ;
#17618 = DIRECTION ( 'NONE',  ( -1.000000000000000000, -0.000000000000000000, -0.000000000000000000 ) ) ;
#17619 = AXIS2_PLACEMENT_3D ( 'NONE', #18117, #3679, #2161 ) ;
#17620 = VERTEX_POINT ( 'NONE', #18223 ) ;
#17621 = CARTESIAN_POINT ( 'NONE',  ( 3.950837973638668288, 0.000000000000000000, 0.000000000000000000 ) ) ;
#17622 = CARTESIAN_POINT ( 'NONE',  ( 0.3307726912345216319, -13.74203354050372283, 0.5948952607472158816 ) ) ;
#17623 = ORIENTED_EDGE ( 'NONE', *, *, #11617, .T. ) ;
#17624 = VECTOR ( 'NONE', #8610, 1000.000000000000227 ) ;
#17625 = ORIENTED_EDGE ( 'NONE', *, *, #18263, .F. ) ;
#17626 = CARTESIAN_POINT ( 'NONE',  ( 2.123976203522053297, -15.54801196254785722, -1.531817366691915483 ) ) ;
#17627 = ORIENTED_EDGE ( 'NONE', *, *, #5811, .F. ) ;
#17628 = B_SPLINE_CURVE_WITH_KNOTS ( 'NONE', 3,
 ( #5483, #4160, #14189, #17440, #7224, #15906 ),
 .UNSPECIFIED., .F., .F.,
 ( 4, 2, 4 ),
 ( 0.000000000000000000, 0.001656992708823640335, 0.003313985417647279802 ),
 .UNSPECIFIED. ) ;
#17629 = ORIENTED_EDGE ( 'NONE', *, *, #1459, .T. ) ;
#17630 = EDGE_CURVE ( 'NONE', #12766, #13344, #15171, .T. ) ;
#17631 = CARTESIAN_POINT ( 'NONE',  ( -26.50000000000000711, -12.50000000000000178, -0.5000000000000000000 ) ) ;
#17632 = FILL_AREA_STYLE_COLOUR ( '', #830 ) ;
#17633 = CARTESIAN_POINT ( 'NONE',  ( 16.56872352241294521, -0.009382111268606286789, 0.004564908236400187953 ) ) ;
#17634 = CARTESIAN_POINT ( 'NONE',  ( 0.3137051932979792457, 4.679953077377670745, -12.91601973349265720 ) ) ;
#17635 = CIRCLE ( 'NONE', #5122, 2.500000000000000000 ) ;
#17636 = UNCERTAINTY_MEASURE_WITH_UNIT (LENGTH_MEASURE( 1.000000000000000082E-05 ), #9937, 'distance_accuracy_value', 'NONE');
#17637 = EDGE_CURVE ( 'NONE', #9622, #11775, #14714, .T. ) ;
#17638 = CARTESIAN_POINT ( 'NONE',  ( 0.3058872367615230181, 12.87003593440634930, -4.821066432589193873 ) ) ;
#17639 = CARTESIAN_POINT ( 'NONE',  ( 16.56822296793089322, 0.009847136207495308519, -0.002414375228568875487 ) ) ;
#17640 = B_SPLINE_CURVE_WITH_KNOTS ( 'NONE', 3,
 ( #15819, #5491, #1099, #8557, #11251, #6950, #17345, #2800, #8648, #12573, #14475, #1388, #3974 ),
 .UNSPECIFIED., .F., .F.,
 ( 4, 3, 3, 3, 4 ),
 ( 2.168404344971008868E-18, 0.0002299780670421057124, 0.0004599561239687910961, 0.0006896788984287892561, 0.0009194956271626406052 ),
 .UNSPECIFIED. ) ;
#17641 = CARTESIAN_POINT ( 'NONE',  ( 2.123976203522053297, -10.37815841598499667, 11.67822624909921814 ) ) ;
#17642 = CARTESIAN_POINT ( 'NONE',  ( -30.00000000000000711, 20.00000000000000000, 0.000000000000000000 ) ) ;
#17643 = CARTESIAN_POINT ( 'NONE',  ( 0.4862570985993235340, 7.559321496869426227, 11.67702470553367711 ) ) ;
#17644 = CARTESIAN_POINT ( 'NONE',  ( 3.950837973638675393, -6.888253895133384930, 12.81214529934972823 ) ) ;
#17645 = CARTESIAN_POINT ( 'NONE',  ( 8.522092701127531811, 5.397361180353144050, 4.388629235579598387 ) ) ;
#17646 = CARTESIAN_POINT ( 'NONE',  ( 0.3095370825347224519, -13.73357284481724427, -0.4597470195091612477 ) ) ;
#17647 = ORIENTED_EDGE ( 'NONE', *, *, #18010, .F. ) ;
#17648 = AXIS2_PLACEMENT_3D ( 'NONE', #5939, #7204, #10442 ) ;
#17649 = VERTEX_POINT ( 'NONE', #2088 ) ;
#17650 = ORIENTED_EDGE ( 'NONE', *, *, #4582, .T. ) ;
#17651 = EDGE_LOOP ( 'NONE', ( #9142, #8966 ) ) ;
#17652 = CARTESIAN_POINT ( 'NONE',  ( 0.3151928476913555821, 0.0002082997483780314805, 13.73922860838472104 ) ) ;
#17653 = DIRECTION ( 'NONE',  ( -6.938893903907228378E-16, -1.000000000000000000, 0.000000000000000000 ) ) ;
#17654 =( BOUNDED_SURFACE ( )  B_SPLINE_SURFACE ( 3, 1, ( 
 ( #3486, #16685 ),
 ( #2070, #12199 ),
 ( #5113, #7910 ),
 ( #6652, #13623 ) ),
 .UNSPECIFIED., .F., .F., .T. ) 
 B_SPLINE_SURFACE_WITH_KNOTS ( ( 4, 4 ),
 ( 2, 2 ),
 ( 0.000000000000000000, 1.000000000000000000 ),
 ( 0.000000000000000000, 1.000000000000000000 ),
 .UNSPECIFIED. ) 
 GEOMETRIC_REPRESENTATION_ITEM ( )  RATIONAL_B_SPLINE_SURFACE ( (
 ( 1.000000000000000000, 1.000000000000000000),
 ( 0.9933953342250438912, 0.8357391271907739227),
 ( 0.9933953342250438912, 0.8357391271907739227),
 ( 1.000000000000000000, 1.000000000000000000) ) ) 
 REPRESENTATION_ITEM ( '' )  SURFACE ( )  );
#17655 =( BOUNDED_SURFACE ( )  B_SPLINE_SURFACE ( 3, 1, ( 
 ( #9536, #12497 ),
 ( #12231, #6773 ),
 ( #9453, #3797 ),
 ( #18147, #12582 ) ),
 .UNSPECIFIED., .F., .F., .T. ) 
 B_SPLINE_SURFACE_WITH_KNOTS ( ( 4, 4 ),
 ( 2, 2 ),
 ( 0.000000000000000000, 1.000000000000000000 ),
 ( 0.000000000000000000, 1.000000000000000000 ),
 .UNSPECIFIED. ) 
 GEOMETRIC_REPRESENTATION_ITEM ( )  RATIONAL_B_SPLINE_SURFACE ( (
 ( 1.000000000000000000, 1.000000000000000000),
 ( 0.7792777138730158093, 0.9689936506012928330),
 ( 0.7792777138730158093, 0.9689936506012928330),
 ( 1.000000000000000000, 1.000000000000000000) ) ) 
 REPRESENTATION_ITEM ( '' )  SURFACE ( )  );
#17656 = B_SPLINE_CURVE_WITH_KNOTS ( 'NONE', 3,
 ( #4952, #18137, #6671, #2094, #5037, #8016 ),
 .UNSPECIFIED., .F., .F.,
 ( 4, 2, 4 ),
 ( 0.000000000000000000, 0.001500839035891551572, 0.003001678071783103145 ),
 .UNSPECIFIED. ) ;
#17657 = CARTESIAN_POINT ( 'NONE',  ( 5.000000000000006217, -30.00000000000000000, 31.00000000000000000 ) ) ;
#17658 = TOROIDAL_SURFACE ( 'NONE', #15812, 2.699999999999999734, 0.2000000000000000111 ) ;
#17659 = VERTEX_POINT ( 'NONE', #457 ) ;
#17660 = CARTESIAN_POINT ( 'NONE',  ( 8.438534575730034959, 1.899950616255187352, 6.598402093327886853 ) ) ;
#17661 = EDGE_CURVE ( 'NONE', #622, #5848, #8528, .T. ) ;
#17662 = EDGE_CURVE ( 'NONE', #748, #14283, #16648, .T. ) ;
#17663 = CARTESIAN_POINT ( 'NONE',  ( -32.49999999999999289, -12.50000000000000178, 0.000000000000000000 ) ) ;
#17664 = ADVANCED_FACE ( 'NONE', ( #18127 ), #5624, .F. ) ;
#17665 = CARTESIAN_POINT ( 'NONE',  ( 2.002547531651519996, 0.6781519942171739812, 12.57989064830759851 ) ) ;
#17666 = CARTESIAN_POINT ( 'NONE',  ( 16.56872352241294521, -0.004907101719994693724, 0.009207754980063731845 ) ) ;
#17667 = CARTESIAN_POINT ( 'NONE',  ( 0.3151928476913540278, 8.075884471919755114, 11.11514699826553176 ) ) ;
#17668 = B_SPLINE_CURVE_WITH_KNOTS ( 'NONE', 3,
 ( #9420, #17936, #719, #16499, #3387, #633 ),
 .UNSPECIFIED., .F., .F.,
 ( 4, 2, 4 ),
 ( 2.790109556687801444E-18, 0.0002017457492448089095, 0.0004034914984896150001 ),
 .UNSPECIFIED. ) ;
#17669 = CARTESIAN_POINT ( 'NONE',  ( 1.847426409206450959, 1.966388007708274189E-11, -12.44303504652081038 ) ) ;
#17670 = CARTESIAN_POINT ( 'NONE',  ( 0.000000000000000000, 0.8660254037844389297, -1.500000000000000000 ) ) ;
#17671 = B_SPLINE_CURVE_WITH_KNOTS ( 'NONE', 3,
 ( #2681, #7196, #1547, #8808 ),
 .UNSPECIFIED., .F., .F.,
 ( 4, 4 ),
 ( 5.784724088816010014E-17, 0.002004993803842651783 ),
 .UNSPECIFIED. ) ;
#17672 = CARTESIAN_POINT ( 'NONE',  ( 0.3150686449036074754, -11.20479228691391604, -7.951193823202520328 ) ) ;
#17673 = CARTESIAN_POINT ( 'NONE',  ( 0.3150686449036065317, -8.199336701264455129, -11.02450593298027570 ) ) ;
#17674 = ORIENTED_EDGE ( 'NONE', *, *, #14106, .F. ) ;
#17675 = EDGE_CURVE ( 'NONE', #17983, #11605, #12651, .T. ) ;
#17676 = VERTEX_POINT ( 'NONE', #6386 ) ;
#17677 = ORIENTED_EDGE ( 'NONE', *, *, #15182, .F. ) ;
#17678 = ORIENTED_EDGE ( 'NONE', *, *, #5449, .F. ) ;
#17679 = ADVANCED_BREP_SHAPE_REPRESENTATION ( '', ( #16668, #2030 ), #5983 ) ;
#17680 = CARTESIAN_POINT ( 'NONE',  ( 1.861628059977118888, 9.751736252960505169, 7.751680370224894645 ) ) ;
#17681 = ORIENTED_EDGE ( 'NONE', *, *, #10761, .T. ) ;
#17682 = CARTESIAN_POINT ( 'NONE',  ( 2.320520222538116961, 10.64885284335071169, -11.60169517779341852 ) ) ;
#17683 = CARTESIAN_POINT ( 'NONE',  ( 16.56679352167444819, 0.008252760440870499439, 0.004277682826582289259 ) ) ;
#17684 = DIRECTION ( 'NONE',  ( 0.000000000000000000, 0.000000000000000000, 1.000000000000000000 ) ) ;
#17685 = PLANE ( 'NONE',  #17870 ) ;
#17686 = EDGE_LOOP ( 'NONE', ( #4339, #5980, #9162, #908 ) ) ;
#17687 = CARTESIAN_POINT ( 'NONE',  ( -5.934112841480000178, 7.499999999999999112, -16.97589560338757408 ) ) ;
#17688 = CARTESIAN_POINT ( 'NONE',  ( 16.56753206892534891, 0.008490833999798923920, 0.004253784598196209618 ) ) ;
#17689 = CARTESIAN_POINT ( 'NONE',  ( 1.846822687350018644, -10.23524390843944687, 7.075150813727085541 ) ) ;
#17690 = ADVANCED_FACE ( 'NONE', ( #7924 ), #3861, .F. ) ;
#17691 = CARTESIAN_POINT ( 'NONE',  ( 2.320521194582547242, 1.795798718313595055, 15.64520804578271118 ) ) ;
#17692 = CARTESIAN_POINT ( 'NONE',  ( 1.560000000000000053, 0.000000000000000000, 1.500000000000000000 ) ) ;
#17693 = EDGE_CURVE ( 'NONE', #17138, #6541, #8100, .T. ) ;
#17694 = CARTESIAN_POINT ( 'NONE',  ( 0.3095370825347224519, 10.84046130709070788, -8.444334731363888125 ) ) ;
#17695 = ORIENTED_EDGE ( 'NONE', *, *, #15551, .T. ) ;
#17696 = B_SPLINE_CURVE_WITH_KNOTS ( 'NONE', 3,
 ( #14621, #10232, #7, #14716, #13477, #392 ),
 .UNSPECIFIED., .F., .F.,
 ( 4, 2, 4 ),
 ( 7.047314121155778821E-19, 0.001657017934710171237, 0.003314035869420342041 ),
 .UNSPECIFIED. ) ;
#17697 = CIRCLE ( 'NONE', #10988, 8.767949192431123251 ) ;
#17698 = CARTESIAN_POINT ( 'NONE',  ( 3.950837973638676281, -6.888253895133199300, -12.81214529934982949 ) ) ;
#17699 = VECTOR ( 'NONE', #1454, 1000.000000000000000 ) ;
#17701 = ORIENTED_EDGE ( 'NONE', *, *, #7282, .F. ) ;
#17700 = CARTESIAN_POINT ( 'NONE',  ( 0.3151928476913555821, 0.0002082997483780314805, 13.73922860838472104 ) ) ;
#17702 = CARTESIAN_POINT ( 'NONE',  ( -112.9592833967653149, -82.42962774651277869, -85.91158569379400944 ) ) ;
#17703 = ADVANCED_FACE ( 'NONE', ( #827 ), #12942, .F. ) ;
#17704 = CARTESIAN_POINT ( 'NONE',  ( 0.3170788640506440603, 8.200855617524691610, -11.02668139258432944 ) ) ;
#17705 = STYLED_ITEM ( 'NONE', ( #18196 ), #3589 ) ;
#17706 = ORIENTED_EDGE ( 'NONE', *, *, #3713, .F. ) ;
#17707 = LINE ( 'NONE', #7477, #14474 ) ;
#17708 = CARTESIAN_POINT ( 'NONE',  ( 4.576598828870276137, -7.499999999999999112, -13.14213029402371014 ) ) ;
#17709 = ORIENTED_EDGE ( 'NONE', *, *, #10072, .F. ) ;
#17710 = CARTESIAN_POINT ( 'NONE',  ( 0.3095370825347224519, 12.91933430393614302, -4.681152801286025955 ) ) ;
#17711 = DIRECTION ( 'NONE',  ( -1.000000000000000000, -0.000000000000000000, -0.000000000000000000 ) ) ;
#17712 = CARTESIAN_POINT ( 'NONE',  ( 2.636624412714756005, -2.161493821597335607, 15.91454522070219113 ) ) ;
#17713 = CARTESIAN_POINT ( 'NONE',  ( 18.75000000000000000, 0.000000000000000000, 0.000000000000000000 ) ) ;
#17714 = EDGE_CURVE ( 'NONE', #1370, #6249, #7031, .T. ) ;
#17715 = VERTEX_POINT ( 'NONE', #6756 ) ;
#17716 = CARTESIAN_POINT ( 'NONE',  ( 16.56753206892534891, -0.006669401563384967299, 0.006760771273036151469 ) ) ;
#17717 = FACE_OUTER_BOUND ( 'NONE', #17158, .T. ) ;
#17718 = CARTESIAN_POINT ( 'NONE',  ( 0.4754618798421162973, -5.007009103465161814, -12.98792082933649539 ) ) ;
#17719 = CARTESIAN_POINT ( 'NONE',  ( 3.950837973638677170, 12.81214529934985080, -6.888253895133152227 ) ) ;
#17720 = CARTESIAN_POINT ( 'NONE',  ( -5.000000000000000000, 20.00000000000000000, 8.000000000000000000 ) ) ;
#17721 = ORIENTED_EDGE ( 'NONE', *, *, #1241, .T. ) ;
#17722 = CARTESIAN_POINT ( 'NONE',  ( 2.123976203522053741, -7.899625852120303549, 13.47898556379310087 ) ) ;
#17723 = LINE ( 'NONE', #3268, #6325 ) ;
#17724 = ORIENTED_EDGE ( 'NONE', *, *, #13421, .F. ) ;
#17725 = ADVANCED_FACE ( 'NONE', ( #5403 ), #18157, .F. ) ;
#17726 = EDGE_LOOP ( 'NONE', ( #4270, #3872, #17262, #5755 ) ) ;
#17727 = DIRECTION ( 'NONE',  ( 1.000000000000000000, 0.000000000000000000, 0.000000000000000000 ) ) ;
#17728 = ORIENTED_EDGE ( 'NONE', *, *, #14818, .F. ) ;
#17729 = CARTESIAN_POINT ( 'NONE',  ( 2.002547531651519996, -12.17374746633580784, 3.242439124566603326 ) ) ;
#17730 = ORIENTED_EDGE ( 'NONE', *, *, #15789, .T. ) ;
#17731 = CARTESIAN_POINT ( 'NONE',  ( 0.3058872367615226295, 13.72992299905060065, 0.6080468242581433813 ) ) ;
#17732 = CARTESIAN_POINT ( 'NONE',  ( 16.56753206892534891, 0.008432171035096382855, 0.004368917149004273269 ) ) ;
#17733 = DIRECTION ( 'NONE',  ( 0.000000000000000000, 0.000000000000000000, 1.000000000000000000 ) ) ;
#17734 = CARTESIAN_POINT ( 'NONE',  ( 0.3151928476913582466, 4.245853234426384404, 13.06671852871090778 ) ) ;
#17735 = DIRECTION ( 'NONE',  ( 1.000000000000000000, 1.239088197126290570E-16, -0.000000000000000000 ) ) ;
#17736 = DIRECTION ( 'NONE',  ( -1.000000000000000000, -0.000000000000000000, -0.000000000000000000 ) ) ;
#17737 =( BOUNDED_SURFACE ( )  B_SPLINE_SURFACE ( 3, 1, ( 
 ( #14470, #8840 ),
 ( #1383, #5767 ),
 ( #10370, #2796 ),
 ( #11611, #1283 ) ),
 .UNSPECIFIED., .F., .F., .T. ) 
 B_SPLINE_SURFACE_WITH_KNOTS ( ( 4, 4 ),
 ( 2, 2 ),
 ( 0.000000000000000000, 1.000000000000000000 ),
 ( 0.000000000000000000, 1.000000000000000000 ),
 .UNSPECIFIED. ) 
 GEOMETRIC_REPRESENTATION_ITEM ( )  RATIONAL_B_SPLINE_SURFACE ( (
 ( 1.000000000000000000, 1.000000000000000000),
 ( 0.9593108457356467333, 0.9995965569486454649),
 ( 0.9593108457356467333, 0.9995965569486454649),
 ( 1.000000000000000000, 1.000000000000000000) ) ) 
 REPRESENTATION_ITEM ( '' )  SURFACE ( )  );
#17738 = DIRECTION ( 'NONE',  ( 0.000000000000000000, 0.000000000000000000, 1.000000000000000000 ) ) ;
#17739 = DIRECTION ( 'NONE',  ( 0.000000000000000000, -1.000000000000000000, 0.000000000000000000 ) ) ;
#17740 = CARTESIAN_POINT ( 'NONE',  ( 1.846138399168762101, 6.971848976711159551, -10.30487220521562541 ) ) ;
#17741 = CARTESIAN_POINT ( 'NONE',  ( 3.512766787570759330, -7.127386085302901186, 13.25664064834469968 ) ) ;
#17742 = EDGE_CURVE ( 'NONE', #5687, #4624, #18396, .T. ) ;
#17743 = AXIS2_PLACEMENT_3D ( 'NONE', #3308, #9150, #14973 ) ;
#17744 = DIRECTION ( 'NONE',  ( 0.000000000000000000, 0.000000000000000000, 1.000000000000000000 ) ) ;
#17745 = CARTESIAN_POINT ( 'NONE',  ( 0.3720661004400037664, -0.7231997263365766981, 13.79610186261029448 ) ) ;
#17746 = ORIENTED_EDGE ( 'NONE', *, *, #3927, .F. ) ;
#17747 = B_SPLINE_CURVE_WITH_KNOTS ( 'NONE', 3,
 ( #6407, #10616, #4683, #3228, #17781, #7564, #3129, #12043, #4967, #9264, #12236, #3331, #18062 ),
 .UNSPECIFIED., .F., .F.,
 ( 4, 3, 3, 3, 4 ),
 ( 1.734723475976807094E-18, 0.0002299780670421060647, 0.0004599561239687893072, 0.0006896788984287890393, 0.0009194956271626404968 ),
 .UNSPECIFIED. ) ;
#17748 = ORIENTED_EDGE ( 'NONE', *, *, #664, .T. ) ;
#17749 = ORIENTED_EDGE ( 'NONE', *, *, #12931, .T. ) ;
#17750 = VERTEX_POINT ( 'NONE', #15616 ) ;
#17751 = CARTESIAN_POINT ( 'NONE',  ( 2.353870697619110164, -3.268530966681543859, -12.53036919722787879 ) ) ;
#17752 = CARTESIAN_POINT ( 'NONE',  ( 0.000000000000000000, 0.8660254037844389297, 1.500000000000000000 ) ) ;
#17753 = CARTESIAN_POINT ( 'NONE',  ( 1.918918678667046684, -7.860057224348774518, -9.738328798462466906 ) ) ;
#17754 = ORIENTED_EDGE ( 'NONE', *, *, #14925, .T. ) ;
#17755 = CYLINDRICAL_SURFACE ( 'NONE', #145, 2.600000000000039613 ) ;
#17756 = DIRECTION ( 'NONE',  ( -0.000000000000000000, -0.000000000000000000, 1.000000000000000000 ) ) ;
#17757 = VECTOR ( 'NONE', #2135, 1000.000000000000000 ) ;
#17758 = CARTESIAN_POINT ( 'NONE',  ( 2.369999999999999662, 5.817072295949927426E-16, -4.750000000000000000 ) ) ;
#17759 = CARTESIAN_POINT ( 'NONE',  ( 0.3095370825347233956, -4.681152801286073917, -12.91933430393612525 ) ) ;
#17760 = CARTESIAN_POINT ( 'NONE',  ( 1.846955891736114852, 12.44001089941741611, -0.2634721419535633880 ) ) ;
#17761 = CARTESIAN_POINT ( 'NONE',  ( 2.636624412714236865, 0.000000000000000000, 0.000000000000000000 ) ) ;
#17762 = CARTESIAN_POINT ( 'NONE',  ( -19.99999999999999645, 2.499999999999998668, -16.99999999999999645 ) ) ;
#17763 = CARTESIAN_POINT ( 'NONE',  ( 0.3148213771069329203, -10.97836617636219181, -8.260246460850838801 ) ) ;
#17764 =( NAMED_UNIT ( * ) PLANE_ANGLE_UNIT ( ) SI_UNIT ( $, .RADIAN. ) );
#17765 = CARTESIAN_POINT ( 'NONE',  ( 0.3150692679895985560, 4.391039771493846722, -13.01874238516605331 ) ) ;
#17766 = ORIENTED_EDGE ( 'NONE', *, *, #6998, .T. ) ;
#17767 = PRODUCT_DEFINITION_SHAPE ( 'NONE', 'NONE',  #1471 ) ;
#17768 = ORIENTED_EDGE ( 'NONE', *, *, #8646, .T. ) ;
#17769 = EDGE_CURVE ( 'NONE', #12252, #6964, #3517, .T. ) ;
#17770 = EDGE_LOOP ( 'NONE', ( #7170, #3316, #2758, #12299 ) ) ;
#17771 = ORIENTED_EDGE ( 'NONE', *, *, #16834, .T. ) ;
#17772 = CARTESIAN_POINT ( 'NONE',  ( 2.636624412714236865, 0.000000000000000000, 0.000000000000000000 ) ) ;
#17773 = VERTEX_POINT ( 'NONE', #5304 ) ;
#17774 = CARTESIAN_POINT ( 'NONE',  ( 1.959212340397945562, -6.829000156128106624, -10.53510106265289359 ) ) ;
#17775 = CARTESIAN_POINT ( 'NONE',  ( 1.846822687350018422, 11.74004266906804617, 4.121816957446238661 ) ) ;
#17776 = CARTESIAN_POINT ( 'NONE',  ( 16.56872352241294521, -0.009207754980064163791, 0.004907101719995779661 ) ) ;
#17777 = AXIS2_PLACEMENT_3D ( 'NONE', #1520, #14509, #16238 ) ;
#17778 = CARTESIAN_POINT ( 'NONE',  ( 8.522092701127531811, 2.505958102592713121, -6.489356537178164075 ) ) ;
#17779 = ORIENTED_EDGE ( 'NONE', *, *, #2332, .T. ) ;
#17780 = CARTESIAN_POINT ( 'NONE',  ( 1.847168016377981781, -3.666915430942684129, 11.89018175117593934 ) ) ;
#17781 = CARTESIAN_POINT ( 'NONE',  ( 0.3150692679895996107, 13.01874238516610482, 4.391039771493711719 ) ) ;
#17782 = DIRECTION ( 'NONE',  ( -1.000000000000000000, 0.000000000000000000, 0.000000000000000000 ) ) ;
#17783 = CARTESIAN_POINT ( 'NONE',  ( 0.3095370825347234511, 12.91933430393608084, 4.681152801286207144 ) ) ;
#17784 = CARTESIAN_POINT ( 'NONE',  ( 1.254255976357135038, 3.563435620217683120, 14.24071337840730322 ) ) ;
#17785 = LINE ( 'NONE', #7758, #3157 ) ;
#17786 = CARTESIAN_POINT ( 'NONE',  ( 15.00000000000000711, -19.99999999999999645, 3.000000000000000000 ) ) ;
#17787 = ORIENTED_EDGE ( 'NONE', *, *, #434, .F. ) ;
#17788 = B_SPLINE_CURVE_WITH_KNOTS ( 'NONE', 3,
 ( #13322, #2985, #6363, #430, #7801, #534 ),
 .UNSPECIFIED., .F., .F.,
 ( 4, 2, 4 ),
 ( 2.622335209753013447E-18, 0.0002017457492448088824, 0.0004034914984896151085 ),
 .UNSPECIFIED. ) ;
#17789 = VECTOR ( 'NONE', #1376, 1000.000000000000000 ) ;
#17790 = CARTESIAN_POINT ( 'NONE',  ( -112.9592833967653149, -82.42962774651277869, -85.91158569379400944 ) ) ;
#17792 = VERTEX_POINT ( 'NONE', #4062 ) ;
#17791 = DIRECTION ( 'NONE',  ( 0.000000000000000000, 0.000000000000000000, 1.000000000000000000 ) ) ;
#17793 = EDGE_CURVE ( 'NONE', #6897, #16688, #12661, .T. ) ;
#17794 = CARTESIAN_POINT ( 'NONE',  ( 3.377929128793395908, -13.92579934231096495, 1.296196549818894539 ) ) ;
#17795 = ADVANCED_FACE ( 'NONE', ( #5484, #12845 ), #9880, .F. ) ;
#17796 = ADVANCED_FACE ( 'NONE', ( #2707 ), #10536, .T. ) ;
#17797 = CARTESIAN_POINT ( 'NONE',  ( 16.56872352241294521, -0.007240717549633941472, -0.007512283835804289302 ) ) ;
#17798 = STYLED_ITEM ( 'NONE', ( #10998 ), #10500 ) ;
#17799 = ORIENTED_EDGE ( 'NONE', *, *, #11732, .T. ) ;
#17800 = CARTESIAN_POINT ( 'NONE',  ( 0.4385251269669958596, -12.93791070501030660, -4.978066129061825329 ) ) ;
#17801 = FACE_OUTER_BOUND ( 'NONE', #1582, .T. ) ;
#17802 = ORIENTED_EDGE ( 'NONE', *, *, #4644, .T. ) ;
#17803 = CARTESIAN_POINT ( 'NONE',  ( 0.4754618798421171855, 7.564402563418640035, -11.68486377711958291 ) ) ;
#17804 = APPLICATION_CONTEXT ( 'automotive_design' ) ;
#17805 = DIRECTION ( 'NONE',  ( -0.7561779333270775005, -0.6322161072786931513, -0.1688126975276622865 ) ) ;
#17806 = CARTESIAN_POINT ( 'NONE',  ( 1.342453679581834924, 13.74702459364891993, -5.476372339889874041 ) ) ;
#17807 = VERTEX_POINT ( 'NONE', #11151 ) ;
#17808 = CONICAL_SURFACE ( 'NONE', #17174, 14.54644660717763927, 0.8559913436420816257 ) ;
#17809 = CARTESIAN_POINT ( 'NONE',  ( 2.123976203522053297, -13.47898556379318435, 7.899625852120161440 ) ) ;
#17810 = DIRECTION ( 'NONE',  ( 0.000000000000000000, 0.000000000000000000, 1.000000000000000000 ) ) ;
#17811 = CARTESIAN_POINT ( 'NONE',  ( 16.56753206892534891, 0.006669401563385194548, 0.006760771273035138390 ) ) ;
#17812 = CARTESIAN_POINT ( 'NONE',  ( 0.4862570985993252548, 11.67702470553365401, 7.559321496869467971 ) ) ;
#17813 = DIRECTION ( 'NONE',  ( -0.000000000000000000, -0.000000000000000000, -1.000000000000000000 ) ) ;
#17814 = EDGE_LOOP ( 'NONE', ( #2719, #11979, #3467, #11766, #9021 ) ) ;
#17815 = CARTESIAN_POINT ( 'NONE',  ( 0.3137051932979809665, -3.805684345189881856, 13.20008686438104739 ) ) ;
#17816 = DIRECTION ( 'NONE',  ( -1.000000000000000000, 0.000000000000000000, 0.000000000000000000 ) ) ;
#17817 = ORIENTED_EDGE ( 'NONE', *, *, #12794, .F. ) ;
#17818 = EDGE_LOOP ( 'NONE', ( #4170, #1521, #12815, #9006 ) ) ;
#17819 = DIRECTION ( 'NONE',  ( -1.000000000000000000, 0.000000000000000000, 0.000000000000000000 ) ) ;
#17820 = EDGE_CURVE ( 'NONE', #11554, #14601, #3780, .T. ) ;
#17821 = ORIENTED_EDGE ( 'NONE', *, *, #3677, .T. ) ;
#17822 = CARTESIAN_POINT ( 'NONE',  ( -30.00000000000000355, -12.50000000000000178, 3.000000000000000000 ) ) ;
#17823 = EDGE_LOOP ( 'NONE', ( #10879, #12576, #5278 ) ) ;
#17824 = VECTOR ( 'NONE', #6619, 1000.000000000000000 ) ;
#17825 = VECTOR ( 'NONE', #4031, 1000.000000000000114 ) ;
#17826 =( LENGTH_UNIT ( ) NAMED_UNIT ( * ) SI_UNIT ( .MILLI., .METRE. ) );
#17827 = CARTESIAN_POINT ( 'NONE',  ( 0.4754618798421162973, -13.89949764182683190, 0.7484603771383941950 ) ) ;
#17828 = CARTESIAN_POINT ( 'NONE',  ( -5.000000000000000000, 6.123233995736766282E-16, 7.000000000000000000 ) ) ;
#17829 = CARTESIAN_POINT ( 'NONE',  ( 1.977228804423231345, 7.806978995470744032, -13.27756617201399969 ) ) ;
#17830 = CYLINDRICAL_SURFACE ( 'NONE', #12067, 5.000000000000049738 ) ;
#17831 = DIRECTION ( 'NONE',  ( 0.000000000000000000, 0.000000000000000000, -1.000000000000000000 ) ) ;
#17832 = CARTESIAN_POINT ( 'NONE',  ( 0.3095370825347234511, -4.681152801286254217, 12.91933430393606486 ) ) ;
#17833 = DIRECTION ( 'NONE',  ( 1.000000000000000000, 0.000000000000000000, 0.000000000000000000 ) ) ;
#17834 = CARTESIAN_POINT ( 'NONE',  ( 0.3095370825347224519, -11.38092634279633941, 7.700448427571837229 ) ) ;
#17835 = CARTESIAN_POINT ( 'NONE',  ( 0.4754618798421167414, -12.98792082933641012, -5.007009103465385635 ) ) ;
#17836 = AXIS2_PLACEMENT_3D ( 'NONE', #10775, #9925, #8685 ) ;
#17837 = AXIS2_PLACEMENT_3D ( 'NONE', #9910, #11548, #9730 ) ;
#17838 = FACE_OUTER_BOUND ( 'NONE', #2655, .T. ) ;
#17839 = ADVANCED_FACE ( 'NONE', ( #1281 ), #7045, .F. ) ;
#17840 = ORIENTED_EDGE ( 'NONE', *, *, #6489, .T. ) ;
#17841 = ORIENTED_EDGE ( 'NONE', *, *, #17028, .T. ) ;
#17842 = EDGE_CURVE ( 'NONE', #12032, #16368, #14045, .T. ) ;
#17843 = ORIENTED_EDGE ( 'NONE', *, *, #14672, .F. ) ;
#17844 = ORIENTED_EDGE ( 'NONE', *, *, #9482, .F. ) ;
#17845 = CARTESIAN_POINT ( 'NONE',  ( 3.664313757352975376, -2.831308606787148463, -13.97913389346637025 ) ) ;
#17846 = DIRECTION ( 'NONE',  ( 1.000000000000000000, 0.000000000000000000, 0.000000000000000000 ) ) ;
#17847 = CARTESIAN_POINT ( 'NONE',  ( 3.950837973638675393, -13.10350451991835818, -6.316429227969608817 ) ) ;
#17848 =( BOUNDED_SURFACE ( )  B_SPLINE_SURFACE ( 3, 1, ( 
 ( #14457, #12745 ),
 ( #1467, #7213 ),
 ( #1183, #15893 ),
 ( #17425, #18574 ) ),
 .UNSPECIFIED., .F., .F., .T. ) 
 B_SPLINE_SURFACE_WITH_KNOTS ( ( 4, 4 ),
 ( 2, 2 ),
 ( 0.000000000000000000, 1.000000000000000000 ),
 ( 0.000000000000000000, 1.000000000000000000 ),
 .UNSPECIFIED. ) 
 GEOMETRIC_REPRESENTATION_ITEM ( )  RATIONAL_B_SPLINE_SURFACE ( (
 ( 1.000000000000000000, 1.000000000000000000),
 ( 0.9933953342250438912, 0.8357391271907739227),
 ( 0.9933953342250438912, 0.8357391271907739227),
 ( 1.000000000000000000, 1.000000000000000000) ) ) 
 REPRESENTATION_ITEM ( '' )  SURFACE ( )  );
#17849 = CARTESIAN_POINT ( 'NONE',  ( 1.136128737974912818E-14, -7.013167318348350499, 27.61316734529538053 ) ) ;
#17850 = DIRECTION ( 'NONE',  ( 0.000000000000000000, 0.000000000000000000, 1.000000000000000000 ) ) ;
#17851 = CARTESIAN_POINT ( 'NONE',  ( 1.959283090834842200, -3.239245055717051791, 12.12982544407804220 ) ) ;
#17852 = CARTESIAN_POINT ( 'NONE',  ( 0.4862570985993235340, -7.559321496869506163, 11.67702470553362559 ) ) ;
#17853 = CARTESIAN_POINT ( 'NONE',  ( 1.847034903785822690, 12.44051878787773191, 0.2299360331934612034 ) ) ;
#17854 = AXIS2_PLACEMENT_3D ( 'NONE', #11120, #8256, #7002 ) ;
#17855 = ADVANCED_FACE ( 'NONE', ( #1093 ), #12756, .T. ) ;
#17856 = CARTESIAN_POINT ( 'NONE',  ( 1.847168016377980670, 11.77471791462004802, -4.022276579849838996 ) ) ;
#17857 = DIRECTION ( 'NONE',  ( -1.000000000000000000, 0.000000000000000000, 6.938893903907227392E-16 ) ) ;
#17858 = DIRECTION ( 'NONE',  ( -1.000000000000000000, 0.000000000000000000, 0.000000000000000000 ) ) ;
#17859 = VECTOR ( 'NONE', #16890, 1000.000000000000000 ) ;
#17860 = CARTESIAN_POINT ( 'NONE',  ( 0.000000000000000000, 0.000000000000000000, 0.000000000000000000 ) ) ;
#17861 = DIRECTION ( 'NONE',  ( 0.000000000000000000, 1.000000000000000000, -0.000000000000000000 ) ) ;
#17862 = ORIENTED_EDGE ( 'NONE', *, *, #9133, .F. ) ;
#17863 = ORIENTED_EDGE ( 'NONE', *, *, #375, .T. ) ;
#17864 = VECTOR ( 'NONE', #3901, 1000.000000000000000 ) ;
#17865 = VERTEX_POINT ( 'NONE', #11803 ) ;
#17866 = CIRCLE ( 'NONE', #9608, 7.000000000000000000 ) ;
#17867 = EDGE_LOOP ( 'NONE', ( #17358, #16569, #15364, #4093 ) ) ;
#17868 = VECTOR ( 'NONE', #13325, 1000.000000000000000 ) ;
#17869 = DIRECTION ( 'NONE',  ( 1.000000000000000000, 0.000000000000000000, 0.000000000000000000 ) ) ;
#17870 = AXIS2_PLACEMENT_3D ( 'NONE', #1327, #9926, #2746 ) ;
#17871 = CARTESIAN_POINT ( 'NONE',  ( 1.254255976357838698, 9.426444230097315469, -11.25336128106935973 ) ) ;
#17872 = DIRECTION ( 'NONE',  ( 0.000000000000000000, 0.000000000000000000, 1.000000000000000000 ) ) ;
#17873 = DIRECTION ( 'NONE',  ( 0.000000000000000000, -1.000000000000000000, 0.000000000000000000 ) ) ;
#17874 = LINE ( 'NONE', #6403, #7811 ) ;
#17875 = VERTEX_POINT ( 'NONE', #7226 ) ;
#17877 = EDGE_CURVE ( 'NONE', #14649, #16909, #3179, .T. ) ;
#17876 = CARTESIAN_POINT ( 'NONE',  ( 2.563381608035277370, 7.500000000000000000, -15.65171369207284435 ) ) ;
#17878 = DIRECTION ( 'NONE',  ( -1.540743955509788340E-33, -1.000000000000000000, -2.533398541561209262E-17 ) ) ;
#17879 = CARTESIAN_POINT ( 'NONE',  ( 16.57778382496167424, 0.01354073047775767452, 0.006312874906843726416 ) ) ;
#17880 = CARTESIAN_POINT ( 'NONE',  ( 0.8740764193765260259, 3.609949042658226581, 13.83508774435983035 ) ) ;
#17881 = EDGE_CURVE ( 'NONE', #10186, #12673, #7321, .T. ) ;
#17882 = CARTESIAN_POINT ( 'NONE',  ( 3.950837973638676281, -14.41405733518059229, -1.958075594453940971 ) ) ;
#17883 = AXIS2_PLACEMENT_3D ( 'NONE', #3644, #4901, #3452 ) ;
#17884 = CIRCLE ( 'NONE', #488, 14.54644660717763927 ) ;
#17885 = CARTESIAN_POINT ( 'NONE',  ( 0.8740779401508858015, -11.05257166392043722, 9.070947476926702890 ) ) ;
#17886 = ORIENTED_EDGE ( 'NONE', *, *, #14180, .F. ) ;
#17887 = CARTESIAN_POINT ( 'NONE',  ( 1.977228804422057395, -11.52787183731166820, 10.21522664410399095 ) ) ;
#17889 = ORIENTED_EDGE ( 'NONE', *, *, #8543, .F. ) ;
#17888 = CARTESIAN_POINT ( 'NONE',  ( 2.002547531651519996, -9.778737580845755062, 7.942910686618138705 ) ) ;
#17890 = FACE_OUTER_BOUND ( 'NONE', #1253, .T. ) ;
#17891 = CARTESIAN_POINT ( 'NONE',  ( 8.438534575730034959, -6.454982381540305347, 2.341351102130253103 ) ) ;
#17892 = ORIENTED_EDGE ( 'NONE', *, *, #16283, .F. ) ;
#17893 = DIRECTION ( 'NONE',  ( 0.000000000000000000, -0.000000000000000000, -1.000000000000000000 ) ) ;
#17894 = CIRCLE ( 'NONE', #14504, 2.600000000000092015 ) ;
#17895 = CARTESIAN_POINT ( 'NONE',  ( -2.826946895707799445, -6.438259034076553533, -12.00000001686866469 ) ) ;
#17896 = ORIENTED_EDGE ( 'NONE', *, *, #11968, .T. ) ;
#17897 = CARTESIAN_POINT ( 'NONE',  ( 1.847380140988742925, 3.740232970470921625, -11.86779270755354432 ) ) ;
#17898 = CARTESIAN_POINT ( 'NONE',  ( 0.3058872367615230181, 13.72992299905060065, -0.6080468242581438254 ) ) ;
#17899 = CARTESIAN_POINT ( 'NONE',  ( 16.56753206892534891, -0.004253784598196824578, -0.008490833999797990639 ) ) ;
#17900 = CARTESIAN_POINT ( 'NONE',  ( 16.57778382496167424, -0.002851818597093308278, -0.01466529584256674387 ) ) ;
#17901 = ADVANCED_FACE ( 'NONE', ( #14469 ), #5863, .F. ) ;
#17902 = EDGE_CURVE ( 'NONE', #11651, #10942, #14960, .T. ) ;
#17903 = ADVANCED_FACE ( 'NONE', ( #1382 ), #15995, .T. ) ;
#17904 = CARTESIAN_POINT ( 'NONE',  ( 1.847380140988738262, -10.00162556679656234, 7.402792205949069171 ) ) ;
#17905 = CARTESIAN_POINT ( 'NONE',  ( 0.4862570985993235340, 7.559321496869593204, -11.67702470553357053 ) ) ;
#17906 = B_SPLINE_CURVE_WITH_KNOTS ( 'NONE', 3,
 ( #12963, #8484, #13062, #7251, #4190, #10103 ),
 .UNSPECIFIED., .F., .F.,
 ( 4, 2, 4 ),
 ( 2.438852479171459636E-18, 0.001657017934711444091, 0.003314035869422886013 ),
 .UNSPECIFIED. ) ;
#17907 = VECTOR ( 'NONE', #7223, 1000.000000000000114 ) ;
#17908 = DIRECTION ( 'NONE',  ( -0.4246593920385850485, -0.1376957914266803973, 0.8948208031649685923 ) ) ;
#17910 = ORIENTED_EDGE ( 'NONE', *, *, #17597, .T. ) ;
#17909 = CARTESIAN_POINT ( 'NONE',  ( 0.000000000000000000, 0.000000000000000000, -6.000000000000000888 ) ) ;
#17911 = CARTESIAN_POINT ( 'NONE',  ( 0.000000000000000000, -0.8660254037844384856, -1.500000000000000000 ) ) ;
#17912 = ORIENTED_EDGE ( 'NONE', *, *, #3209, .F. ) ;
#17913 = CARTESIAN_POINT ( 'NONE',  ( 0.3145729642390363567, -7.825496023201391260, 11.29233589755989797 ) ) ;
#17914 = CARTESIAN_POINT ( 'NONE',  ( 0.3058872367615226295, -13.24582953854928036, 3.664492643742712108 ) ) ;
#17915 = ADVANCED_FACE ( 'NONE', ( #7613 ), #8398, .T. ) ;
#17916 = ORIENTED_EDGE ( 'NONE', *, *, #12774, .T. ) ;
#17917 = ORIENTED_EDGE ( 'NONE', *, *, #16190, .F. ) ;
#17918 = DIRECTION ( 'NONE',  ( 0.9034263296138843602, 0.000000000000000000, 0.4287433579198459133 ) ) ;
#17919 = AXIS2_PLACEMENT_3D ( 'NONE', #9273, #15378, #860 ) ;
#17920 = ORIENTED_EDGE ( 'NONE', *, *, #8809, .T. ) ;
#17921 = CARTESIAN_POINT ( 'NONE',  ( 2.002547531651519996, 3.242439124566649511, 12.17374746633579541 ) ) ;
#17922 = VERTEX_POINT ( 'NONE', #9032 ) ;
#17923 = VECTOR ( 'NONE', #2852, 1000.000000000000227 ) ;
#17924 = DIRECTION ( 'NONE',  ( 0.000000000000000000, -1.000000000000000000, 0.000000000000000000 ) ) ;
#17925 = CARTESIAN_POINT ( 'NONE',  ( 0.3148213771069381384, -13.73693585713733611, -0.2297580318216151940 ) ) ;
#17926 = CARTESIAN_POINT ( 'NONE',  ( -5.000000000000000000, 20.00000000000000000, 7.000000000000000000 ) ) ;
#17927 = CARTESIAN_POINT ( 'NONE',  ( 0.3137051932979792457, -8.442169467526928983, 10.83767969834800127 ) ) ;
#17928 = AXIS2_PLACEMENT_3D ( 'NONE', #6593, #18250, #8390 ) ;
#17929 = DIRECTION ( 'NONE',  ( -1.000000000000000000, -0.000000000000000000, -0.000000000000000000 ) ) ;
#17930 = CARTESIAN_POINT ( 'NONE',  ( 0.3720661004400037664, -3.575426119359092159, -13.34435358167256247 ) ) ;
#17931 = SURFACE_SIDE_STYLE ('',( #716 ) ) ;
#17932 = LINE ( 'NONE', #6455, #8936 ) ;
#17933 = CARTESIAN_POINT ( 'NONE',  ( 1.846138399168762101, -11.69739621335919111, -4.238866729160527314 ) ) ;
#17934 = EDGE_CURVE ( 'NONE', #15231, #2734, #10392, .T. ) ;
#17935 = VECTOR ( 'NONE', #16260, 1000.000000000000000 ) ;
#17936 = CARTESIAN_POINT ( 'NONE',  ( 0.3132635586635982294, 3.740017578711948953, -13.21855946425832684 ) ) ;
#17937 = AXIS2_PLACEMENT_3D ( 'NONE', #2335, #15606, #17228 ) ;
#17938 = CARTESIAN_POINT ( 'NONE',  ( 0.4862570985993235340, -13.89016912371016943, -0.7479633556563904939 ) ) ;
#17939 = AXIS2_PLACEMENT_3D ( 'NONE', #13787, #2224, #2142 ) ;
#17940 = CLOSED_SHELL ( 'NONE', ( #12979, #315, #9406, #7856, #1286, #8290, #13506, #12748, #18746, #10026, #18805, #17436, #5171, #1288, #7930, #9505, #12561, #7954, #17855, #9646, #11019, #13388, #9187, #5287, #294, #17439, #1617 ) ) ;
#17941 = CARTESIAN_POINT ( 'NONE',  ( 1.847380140988742703, -11.86779270755355853, -3.740232970470879881 ) ) ;
#17942 = ORIENTED_EDGE ( 'NONE', *, *, #1120, .F. ) ;
#17943 = EDGE_CURVE ( 'NONE', #2106, #10362, #9611, .T. ) ;
#17944 = ORIENTED_EDGE ( 'NONE', *, *, #3443, .T. ) ;
#17945 = ORIENTED_EDGE ( 'NONE', *, *, #9939, .T. ) ;
#17946 = ORIENTED_EDGE ( 'NONE', *, *, #6158, .F. ) ;
#17947 = CARTESIAN_POINT ( 'NONE',  ( 0.3137051932979792457, -7.698472063774386420, -11.37800749014139612 ) ) ;
#17948 = B_SPLINE_CURVE_WITH_KNOTS ( 'NONE', 3,
 ( #7802, #7992, #2324, #5283, #11129, #3378 ),
 .UNSPECIFIED., .F., .F.,
 ( 4, 2, 4 ),
 ( 1.951563910473907981E-18, 0.0002017457492448081235, 0.0004034914984896142954 ),
 .UNSPECIFIED. ) ;
#17949 = CARTESIAN_POINT ( 'NONE',  ( 0.4862570985993235340, -13.89016912371016943, -0.7479633556563904939 ) ) ;
#17950 = CARTESIAN_POINT ( 'NONE',  ( 2.002547531651519996, -3.242439124566566910, -12.17374746633581495 ) ) ;
#17951 = CARTESIAN_POINT ( 'NONE',  ( 0.4385251269669948049, 13.84299131624729817, 0.7363879510385874516 ) ) ;
#17952 = CARTESIAN_POINT ( 'NONE',  ( 3.950837973638677170, -14.31366178983255466, 2.591948120961746760 ) ) ;
#17953 = ORIENTED_EDGE ( 'NONE', *, *, #18690, .F. ) ;
#17954 = CARTESIAN_POINT ( 'NONE',  ( 1.846138399168762101, -12.43476674860266229, -0.4167076046096845898 ) ) ;
#17955 = CARTESIAN_POINT ( 'NONE',  ( 1.847034903785822690, -11.90269060117936739, 3.625649561595261083 ) ) ;
#17956 = LINE ( 'NONE', #171, #17371 ) ;
#17957 = DIRECTION ( 'NONE',  ( 1.000000000000000000, 0.000000000000000000, 0.000000000000000000 ) ) ;
#17958 = CARTESIAN_POINT ( 'NONE',  ( 2.636624412714237309, 15.80357026013209953, 2.862162146984226663 ) ) ;
#17959 = CARTESIAN_POINT ( 'NONE',  ( 16.56679352167444819, -0.001518074900131792136, -0.009170718284672557674 ) ) ;
#17960 = CARTESIAN_POINT ( 'NONE',  ( 0.3720661004400040439, -11.58636699658209679, -7.524064345033593781 ) ) ;
#17961 = VECTOR ( 'NONE', #12281, 1000.000000000000000 ) ;
#17962 = ORIENTED_EDGE ( 'NONE', *, *, #9134, .F. ) ;
#17963 = ADVANCED_FACE ( 'NONE', ( #17531 ), #18867, .F. ) ;
#17964 = VERTEX_POINT ( 'NONE', #8927 ) ;
#17965 = ORIENTED_EDGE ( 'NONE', *, *, #10100, .F. ) ;
#17966 = ORIENTED_EDGE ( 'NONE', *, *, #4413, .F. ) ;
#17967 = CARTESIAN_POINT ( 'NONE',  ( 1.847461586945729595, -7.341074796295863791, -10.04711372545053116 ) ) ;
#17968 = EDGE_CURVE ( 'NONE', #17143, #14747, #10465, .T. ) ;
#17969 = CARTESIAN_POINT ( 'NONE',  ( 2.697797270744666687, -10.19107313879051269, -8.537712152180978009 ) ) ;
#17970 = CARTESIAN_POINT ( 'NONE',  ( 3.512766787570692273, -2.682019731918297012, -14.81029789862167867 ) ) ;
#17971 = CARTESIAN_POINT ( 'NONE',  ( 2.002547531651519996, -12.57989064830759141, -0.6781519942173057647 ) ) ;
#17972 = CARTESIAN_POINT ( 'NONE',  ( -1.979226605763932723, -14.99999999999999645, 6.000000000000000000 ) ) ;
#17973 = ORIENTED_EDGE ( 'NONE', *, *, #3221, .F. ) ;
#17974 = CARTESIAN_POINT ( 'NONE',  ( 0.3132642857406563452, -0.5276792104583234444, 13.72733058964894326 ) ) ;
#17975 = CARTESIAN_POINT ( 'NONE',  ( 0.000000000000000000, 0.000000000000000000, -12.00000000000000000 ) ) ;
#17976 = CARTESIAN_POINT ( 'NONE',  ( -5.308815406012119986, 7.500000000000000000, -12.96907596528355455 ) ) ;
#17977 = CARTESIAN_POINT ( 'NONE',  ( 3.950837973638677170, -1.958075594453692503, -14.41405733518062959 ) ) ;
#17978 = FILL_AREA_STYLE_COLOUR ( '', #1641 ) ;
#17979 = CARTESIAN_POINT ( 'NONE',  ( 0.3145734862173233393, 13.15783074029284272, -3.953068532979860272 ) ) ;
#17980 = EDGE_LOOP ( 'NONE', ( #4656, #3419, #10261, #4845 ) ) ;
#17981 = CARTESIAN_POINT ( 'NONE',  ( 1.254255976357308233, 13.61551404021196277, 5.487601330834896096 ) ) ;
#17983 = VERTEX_POINT ( 'NONE', #1666 ) ;
#17982 = CARTESIAN_POINT ( 'NONE',  ( 1.847461586945734702, 11.82388984758123840, -3.877048136045254001 ) ) ;
#17984 = CARTESIAN_POINT ( 'NONE',  ( 0.3307726912345234083, 11.46720933246398388, 7.596084275798933305 ) ) ;
#17985 = ADVANCED_FACE ( 'NONE', ( #11900 ), #16300, .T. ) ;
#17986 = CARTESIAN_POINT ( 'NONE',  ( 0.4384471787762801442, 10.76632603192799742, -8.732395932355569101 ) ) ;
#17987 = EDGE_CURVE ( 'NONE', #18610, #16059, #11313, .T. ) ;
#17988 = ORIENTED_EDGE ( 'NONE', *, *, #1790, .T. ) ;
#17989 = CARTESIAN_POINT ( 'NONE',  ( 16.56679352167444819, 0.009190982326619719436, 0.001390132774594471984 ) ) ;
#17990 = CARTESIAN_POINT ( 'NONE',  ( -1.089171355198575775, -7.500000000000000888, -14.58290923294939923 ) ) ;
#17991 = ORIENTED_EDGE ( 'NONE', *, *, #2623, .F. ) ;
#17992 = CARTESIAN_POINT ( 'NONE',  ( 0.3170788640506440603, 13.11595226728163510, -4.100430649997826471 ) ) ;
#17993 = CARTESIAN_POINT ( 'NONE',  ( 2.747332970342022840, -16.17136872824897154, -2.409922051470850146 ) ) ;
#17994 = DIRECTION ( 'NONE',  ( -1.000000000000000000, 0.000000000000000000, 0.000000000000000000 ) ) ;
#17995 = CARTESIAN_POINT ( 'NONE',  ( 3.950837973638676281, -6.316429227969562632, 13.10350451991838128 ) ) ;
#17996 = EDGE_LOOP ( 'NONE', ( #7046, #397, #14136, #11739 ) ) ;
#17997 = VECTOR ( 'NONE', #7006, 1000.000000000000114 ) ;
#17998 = VECTOR ( 'NONE', #17125, 1000.000000000000000 ) ;
#17999 = DIRECTION ( 'NONE',  ( 1.734723475976806848E-16, 1.000000000000000000, -0.000000000000000000 ) ) ;
#18000 = DIRECTION ( 'NONE',  ( -1.000000000000000000, -0.000000000000000000, -0.000000000000000000 ) ) ;
#18002 = VERTEX_POINT ( 'NONE', #12194 ) ;
#18001 = CARTESIAN_POINT ( 'NONE',  ( 2.705023505549863039, -12.36217802824809020, 4.909285963184022883 ) ) ;
#18003 = DIRECTION ( 'NONE',  ( 0.000000000000000000, 0.000000000000000000, 1.000000000000000000 ) ) ;
#18004 = ORIENTED_EDGE ( 'NONE', *, *, #17662, .F. ) ;
#18005 = CARTESIAN_POINT ( 'NONE',  ( 0.3151928476913556376, -8.075547435847033384, 11.11539186930584044 ) ) ;
#18006 = LINE ( 'NONE', #616, #8769 ) ;
#18007 = ORIENTED_EDGE ( 'NONE', *, *, #12587, .F. ) ;
#18008 = EDGE_CURVE ( 'NONE', #2558, #2787, #7484, .T. ) ;
#18009 = ADVANCED_FACE ( 'NONE', ( #17027 ), #1870, .F. ) ;
#18010 = EDGE_CURVE ( 'NONE', #5801, #4529, #18378, .T. ) ;
#18011 = EDGE_LOOP ( 'NONE', ( #10679, #6357, #4763, #15377 ) ) ;
#18012 = ORIENTED_EDGE ( 'NONE', *, *, #2325, .F. ) ;
#18013 = CARTESIAN_POINT ( 'NONE',  ( 2.636624412714236865, 0.000000000000000000, 0.000000000000000000 ) ) ;
#18014 = VERTEX_POINT ( 'NONE', #5360 ) ;
#18015 = CARTESIAN_POINT ( 'NONE',  ( 0.3095370825347224519, 7.700448427571875420, 11.38092634279631099 ) ) ;
#18016 = DIRECTION ( 'NONE',  ( -0.7561779333270775005, 0.6322161072786942615, 0.1688126975276577901 ) ) ;
#18017 = DIRECTION ( 'NONE',  ( 0.000000000000000000, 0.000000000000000000, 1.000000000000000000 ) ) ;
#18018 = CARTESIAN_POINT ( 'NONE',  ( 2.320521194581854907, 15.64520804578206281, -1.795798718312993758 ) ) ;
#18019 = CARTESIAN_POINT ( 'NONE',  ( 2.747332970342022840, 14.63517873738956965, -7.289199830146954717 ) ) ;
#18020 = CARTESIAN_POINT ( 'NONE',  ( 0.3151928479966097374, 1.775918418904422640E-15, 13.73922861026898623 ) ) ;
#18021 = CARTESIAN_POINT ( 'NONE',  ( 1.847426409206450959, 1.966388007708274189E-11, -12.44303504652081038 ) ) ;
#18022 = CARTESIAN_POINT ( 'NONE',  ( 1.342453679581834924, -5.476372339889922003, -13.74702459364890039 ) ) ;
#18023 = CARTESIAN_POINT ( 'NONE',  ( 0.3308579732647004001, 0.5950689966506276241, -13.74211098745268345 ) ) ;
#18024 = CARTESIAN_POINT ( 'NONE',  ( 0.3148213771069364175, 7.888490156175222090, 11.24846294176314387 ) ) ;
#18025 = CARTESIAN_POINT ( 'NONE',  ( 1.254255976357675717, -14.64488542023465101, -1.011593778944541278 ) ) ;
#18026 = CARTESIAN_POINT ( 'NONE',  ( 0.3095370825347224519, 13.20347358821919670, -3.806662003783277459 ) ) ;
#18027 = CARTESIAN_POINT ( 'NONE',  ( 16.56872352241294521, 0.001442253899401802278, 0.01033355228142402403 ) ) ;
#18028 = ORIENTED_EDGE ( 'NONE', *, *, #16193, .F. ) ;
#18029 = ADVANCED_FACE ( 'NONE', ( #14951 ), #17830, .T. ) ;
#18030 = EDGE_CURVE ( 'NONE', #4049, #5922, #15047, .T. ) ;
#18031 = EDGE_CURVE ( 'NONE', #13922, #18593, #18177, .T. ) ;
#18032 = ORIENTED_EDGE ( 'NONE', *, *, #9379, .T. ) ;
#18033 = VERTEX_POINT ( 'NONE', #1965 ) ;
#18034 = ORIENTED_EDGE ( 'NONE', *, *, #8059, .T. ) ;
#18035 = EDGE_CURVE ( 'NONE', #3873, #13478, #10640, .T. ) ;
#18036 = LINE ( 'NONE', #10773, #6608 ) ;
#18037 = CARTESIAN_POINT ( 'NONE',  ( 0.4385251269669978580, 4.978066129061869738, -12.93791070501029239 ) ) ;
#18038 = CARTESIAN_POINT ( 'NONE',  ( 2.705023505549865703, 11.23800170568056878, 7.115606223895208693 ) ) ;
#18039 = PRODUCT_DEFINITION_CONTEXT ( 'detailed design', #826, 'design' ) ;
#18040 = ORIENTED_EDGE ( 'NONE', *, *, #950, .F. ) ;
#18041 = CARTESIAN_POINT ( 'NONE',  ( 16.57605080000000086, 0.000000000000000000, 0.000000000000000000 ) ) ;
#18042 = CARTESIAN_POINT ( 'NONE',  ( 0.4862570985993235340, -11.67702470553370553, 7.559321496869385371 ) ) ;
#18043 = CARTESIAN_POINT ( 'NONE',  ( 2.123976203522053741, 11.67822624909940821, -10.37815841598478883 ) ) ;
#18044 = DIRECTION ( 'NONE',  ( 0.7635533937278216055, -0.6453904417649387604, -0.02138673900302107828 ) ) ;
#18045 = CARTESIAN_POINT ( 'NONE',  ( 2.320520222538102306, -7.743191299716920106, -13.71278186123380927 ) ) ;
#18046 = B_SPLINE_CURVE_WITH_KNOTS ( 'NONE', 3,
 ( #1148, #8509, #9748, #15572 ),
 .UNSPECIFIED., .F., .F.,
 ( 4, 4 ),
 ( 0.000000000000000000, 0.002004993803842713366 ),
 .UNSPECIFIED. ) ;
#18047 = CARTESIAN_POINT ( 'NONE',  ( 0.4754618798421162973, -11.68486377711960955, -7.564402563418597403 ) ) ;
#18048 = ORIENTED_EDGE ( 'NONE', *, *, #962, .T. ) ;
#18049 = SHAPE_REPRESENTATION ( 'straight miter gear_iso_ISO - Straight miter gear 1.5M20T 20PA 2FW ---20O5H16.576MD5.0N', ( #2030 ), #15178 ) ;
#18050 = ORIENTED_EDGE ( 'NONE', *, *, #6993, .F. ) ;
#18051 = ORIENTED_EDGE ( 'NONE', *, *, #18671, .T. ) ;
#18052 = ORIENTED_EDGE ( 'NONE', *, *, #332, .T. ) ;
#18053 = LINE ( 'NONE', #281, #10134 ) ;
#18054 = DIRECTION ( 'NONE',  ( 0.000000000000000000, 0.000000000000000000, 1.000000000000000000 ) ) ;
#18055 = AXIS2_PLACEMENT_3D ( 'NONE', #10487, #16022, #170 ) ;
#18056 = EDGE_CURVE ( 'NONE', #9556, #17715, #3554, .T. ) ;
#18057 = DIRECTION ( 'NONE',  ( -0.5547001962252284812, -0.8320502943378440541, 0.000000000000000000 ) ) ;
#18058 = CARTESIAN_POINT ( 'NONE',  ( 16.56679352167444819, 0.009170718284672562878, -0.001518074900131760043 ) ) ;
#18059 = DIRECTION ( 'NONE',  ( -1.000000000000000000, -0.000000000000000000, -0.000000000000000000 ) ) ;
#18060 = ORIENTED_EDGE ( 'NONE', *, *, #15117, .F. ) ;
#18061 = CARTESIAN_POINT ( 'NONE',  ( 0.1112489676725757909, 7.500000000000000888, -14.17494330110304901 ) ) ;
#18062 = CARTESIAN_POINT ( 'NONE',  ( 0.3137051932979792457, 13.20008686438105983, 3.805684345189833451 ) ) ;
#18063 = CARTESIAN_POINT ( 'NONE',  ( -0.5390158121839171423, 6.982261029182147638, -11.99999999709518761 ) ) ;
#18064 = CARTESIAN_POINT ( 'NONE',  ( 1.846138399168762101, -10.30487220521574976, 6.971848976710974810 ) ) ;
#18065 = B_SPLINE_CURVE_WITH_KNOTS ( 'NONE', 3,
 ( #6274, #6176, #4743, #4552, #13238, #7063 ),
 .UNSPECIFIED., .F., .F.,
 ( 4, 2, 4 ),
 ( 0.000000000000000000, 0.001657017934710632240, 0.003314035869421264480 ),
 .UNSPECIFIED. ) ;
#18066 = DIRECTION ( 'NONE',  ( 0.000000000000000000, 0.000000000000000000, 1.000000000000000000 ) ) ;
#18067 =( NAMED_UNIT ( * ) PLANE_ANGLE_UNIT ( ) SI_UNIT ( $, .RADIAN. ) );
#18068 = CARTESIAN_POINT ( 'NONE',  ( 0.3145734862173240054, 0.3064017202077272128, -13.73540602248380971 ) ) ;
#18069 = B_SPLINE_CURVE_WITH_KNOTS ( 'NONE', 3,
 ( #11758, #11662, #4392, #10417, #9175, #14615 ),
 .UNSPECIFIED., .F., .F.,
 ( 4, 2, 4 ),
 ( 3.303099811781675862E-17, 0.0001825746017570575581, 0.0003651492035140820481 ),
 .UNSPECIFIED. ) ;
#18070 = EDGE_LOOP ( 'NONE', ( #7857, #8400, #5063, #15682 ) ) ;
#18071 = EDGE_CURVE ( 'NONE', #570, #11716, #963, .T. ) ;
#18073 = ORIENTED_EDGE ( 'NONE', *, *, #13966, .T. ) ;
#18072 = FACE_OUTER_BOUND ( 'NONE', #4355, .T. ) ;
#18074 = CARTESIAN_POINT ( 'NONE',  ( 0.3939822652208138098, 12.90851734139308071, 4.930560016699109482 ) ) ;
#18075 = CIRCLE ( 'NONE', #6788, 2.500000000000000000 ) ;
#18076 = EDGE_CURVE ( 'NONE', #6766, #181, #8331, .T. ) ;
#18077 = EDGE_CURVE ( 'NONE', #17471, #13361, #12956, .T. ) ;
#18078 = ORIENTED_EDGE ( 'NONE', *, *, #13090, .T. ) ;
#18079 = CARTESIAN_POINT ( 'NONE',  ( 2.636624412714763555, 6.973567714907159321, 14.46769361191226722 ) ) ;
#18080 = PRODUCT_DEFINITION_SHAPE ( 'NONE', 'NONE',  #18905 ) ;
#18081 = CARTESIAN_POINT ( 'NONE',  ( 0.6292663627305138396, -7.500000000000000888, -14.32718894987486635 ) ) ;
#18082 = ORIENTED_EDGE ( 'NONE', *, *, #6993, .T. ) ;
#18083 = CARTESIAN_POINT ( 'NONE',  ( 1.846138399168762101, 3.446241763653166590, -11.95493567637846866 ) ) ;
#18084 = CARTESIAN_POINT ( 'NONE',  ( 0.3145729642390356351, 13.73540280162741034, -0.3065092323351694126 ) ) ;
#18085 = CARTESIAN_POINT ( 'NONE',  ( 1.861706995891670546, -12.00328602385077659, -3.332865258614104320 ) ) ;
#18086 = DIRECTION ( 'NONE',  ( -1.000000000000000000, 0.000000000000000000, 0.000000000000000000 ) ) ;
#18087 = CIRCLE ( 'NONE', #8317, 7.000000000000000000 ) ;
#18088 = EDGE_CURVE ( 'NONE', #5678, #3563, #10664, .T. ) ;
#18089 = CARTESIAN_POINT ( 'NONE',  ( 1.959212340397961327, 12.53706137681889743, 0.6675998551412224424 ) ) ;
#18090 = DIRECTION ( 'NONE',  ( 1.000000000000000000, 0.000000000000000000, -0.000000000000000000 ) ) ;
#18092 = EDGE_LOOP ( 'NONE', ( #9486, #9699, #12785, #16507 ) ) ;
#18091 = CARTESIAN_POINT ( 'NONE',  ( 2.002547531651519996, 10.57595306287302250, -6.845637710436074386 ) ) ;
#18093 = CARTESIAN_POINT ( 'NONE',  ( 3.950837973638675393, -2.591948120961912849, 14.31366178983252446 ) ) ;
#18094 = EDGE_CURVE ( 'NONE', #12234, #256, #3833, .T. ) ;
#18095 = ORIENTED_EDGE ( 'NONE', *, *, #18806, .T. ) ;
#18096 = CARTESIAN_POINT ( 'NONE',  ( 3.950837973638668288, 0.000000000000000000, 0.000000000000000000 ) ) ;
#18097 = CARTESIAN_POINT ( 'NONE',  ( 0.8740764193768466583, -11.05257066464528748, -9.070946295054149289 ) ) ;
#18098 = ORIENTED_EDGE ( 'NONE', *, *, #15650, .F. ) ;
#18099 = VERTEX_POINT ( 'NONE', #8794 ) ;
#18100 = CARTESIAN_POINT ( 'NONE',  ( -2.750000000000000000, 3.367778697655221012E-16, 11.00000000000000000 ) ) ;
#18101 = EDGE_LOOP ( 'NONE', ( #13367, #7429, #11696, #16801 ) ) ;
#18102 = CARTESIAN_POINT ( 'NONE',  ( 16.56822296793089322, -0.002414375228568911048, -0.009847136207495301580 ) ) ;
#18103 = ORIENTED_EDGE ( 'NONE', *, *, #12367, .F. ) ;
#18104 = CARTESIAN_POINT ( 'NONE',  ( 3.074695600507308946, 2.093687500611960850, 15.41438262616221522 ) ) ;
#18105 = CARTESIAN_POINT ( 'NONE',  ( 0.3137051932979792457, -13.73004976592202375, 0.4596302728639276580 ) ) ;
#18106 = CARTESIAN_POINT ( 'NONE',  ( 0.3137051932979792457, 11.37800749014142276, -7.698472063774345564 ) ) ;
#18107 = CARTESIAN_POINT ( 'NONE',  ( 1.342453679581834924, 13.74702459364891993, -5.476372339889874041 ) ) ;
#18108 = AXIS2_PLACEMENT_3D ( 'NONE', #14274, #1175, #7015 ) ;
#18109 = DIRECTION ( 'NONE',  ( -1.000000000000000000, -0.000000000000000000, -0.000000000000000000 ) ) ;
#18110 = PRODUCT_CONTEXT ( 'NONE', #18754, 'mechanical' ) ;
#18111 = CARTESIAN_POINT ( 'NONE',  ( 16.56872352241294521, -0.01033355228142402750, 0.001442253899401767583 ) ) ;
#18112 = EDGE_CURVE ( 'NONE', #13667, #11517, #12663, .T. ) ;
#18113 = CARTESIAN_POINT ( 'NONE',  ( 2.636624412714236865, 0.000000000000000000, 0.000000000000000000 ) ) ;
#18114 = ADVANCED_BREP_SHAPE_REPRESENTATION ( '', ( #3553, #2030 ), #14825 ) ;
#18115 = CARTESIAN_POINT ( 'NONE',  ( 2.353870697619111496, -8.216087327473003299, 10.00946331859660710 ) ) ;
#18116 = CARTESIAN_POINT ( 'NONE',  ( 0.8740764193766143997, 13.31469591265758545, 5.211550415968988936 ) ) ;
#18117 = CARTESIAN_POINT ( 'NONE',  ( -20.00000000000000000, -2.500000000000000444, -16.99999999999999645 ) ) ;
#18118 = ORIENTED_EDGE ( 'NONE', *, *, #7259, .T. ) ;
#18119 = VECTOR ( 'NONE', #3674, 1000.000000000000000 ) ;
#18120 = ORIENTED_EDGE ( 'NONE', *, *, #17902, .F. ) ;
#18121 = EDGE_LOOP ( 'NONE', ( #8161, #4613, #9815, #13567 ) ) ;
#18122 = ORIENTED_EDGE ( 'NONE', *, *, #5943, .F. ) ;
#18123 =( BOUNDED_SURFACE ( )  B_SPLINE_SURFACE ( 3, 1, ( 
 ( #920, #18775 ),
 ( #6762, #12571 ),
 ( #8556, #18399 ),
 ( #6949, #3973 ) ),
 .UNSPECIFIED., .F., .F., .T. ) 
 B_SPLINE_SURFACE_WITH_KNOTS ( ( 4, 4 ),
 ( 2, 2 ),
 ( 0.000000000000000000, 1.000000000000000000 ),
 ( 0.000000000000000000, 1.000000000000000000 ),
 .UNSPECIFIED. ) 
 GEOMETRIC_REPRESENTATION_ITEM ( )  RATIONAL_B_SPLINE_SURFACE ( (
 ( 1.000000000000000000, 1.000000000000000000),
 ( 0.7792777138730160313, 0.9689936506012927220),
 ( 0.7792777138730160313, 0.9689936506012927220),
 ( 1.000000000000000000, 1.000000000000000000) ) ) 
 REPRESENTATION_ITEM ( '' )  SURFACE ( )  );
#18124 = VERTEX_POINT ( 'NONE', #1436 ) ;
#18125 = CARTESIAN_POINT ( 'NONE',  ( 0.3151926232592466848, 11.16039997398654116, 8.013596737356428079 ) ) ;
#18126 = CARTESIAN_POINT ( 'NONE',  ( 4.478293880065215227, -7.500000000000001776, -16.64373187125687181 ) ) ;
#18127 = FACE_OUTER_BOUND ( 'NONE', #5778, .T. ) ;
#18128 = CARTESIAN_POINT ( 'NONE',  ( 8.438534575730034959, -5.688336279099072357, 3.845978796786017284 ) ) ;
#18129 = EDGE_CURVE ( 'NONE', #2803, #15520, #14337, .T. ) ;
#18130 = DIRECTION ( 'NONE',  ( -1.000000000000000000, -0.000000000000000000, -0.000000000000000000 ) ) ;
#18131 = EDGE_CURVE ( 'NONE', #381, #9516, #11078, .T. ) ;
#18132 = CARTESIAN_POINT ( 'NONE',  ( 3.950837973638676281, -12.81214529934979929, 6.888253895133251703 ) ) ;
#18133 = EDGE_CURVE ( 'NONE', #3596, #2439, #2877, .T. ) ;
#18134 = VECTOR ( 'NONE', #6966, 1000.000000000000227 ) ;
#18135 = CARTESIAN_POINT ( 'NONE',  ( 2.636624412716062515, -6.973567714909003179, -14.46769361191335790 ) ) ;
#18136 = VECTOR ( 'NONE', #1821, 1000.000000000000000 ) ;
#18137 = CARTESIAN_POINT ( 'NONE',  ( 2.353870697619111496, 3.268530966681629568, 12.53036919722785925 ) ) ;
#18138 = ORIENTED_EDGE ( 'NONE', *, *, #14626, .F. ) ;
#18139 = B_SPLINE_CURVE_WITH_KNOTS ( 'NONE', 3,
 ( #8345, #2489, #8428, #18287, #10682, #18373, #1166, #13637, #6640, #6814, #2585, #7004, #14160 ),
 .UNSPECIFIED., .F., .F.,
 ( 4, 3, 3, 3, 4 ),
 ( 2.602085213965210642E-18, 0.0002299780670421064713, 0.0004599561239687913672, 0.0006896788984287877382, 0.0009194956271626401716 ),
 .UNSPECIFIED. ) ;
#18140 = EDGE_LOOP ( 'NONE', ( #7069, #10450, #5845, #11258, #4387, #8983 ) ) ;
#18141 = ORIENTED_EDGE ( 'NONE', *, *, #8438, .T. ) ;
#18142 = VERTEX_POINT ( 'NONE', #5718 ) ;
#18143 = CARTESIAN_POINT ( 'NONE',  ( 2.320521194584406199, 14.32454473830047270, -6.542541239687196253 ) ) ;
#18144 = CARTESIAN_POINT ( 'NONE',  ( 16.57210152137263393, 0.009075239946108201033, -0.01136813053532078656 ) ) ;
#18145 = CIRCLE ( 'NONE', #134, 2.749999999999996891 ) ;
#18146 = CARTESIAN_POINT ( 'NONE',  ( 1.977436885027552549, 15.04044112860454518, -3.321781585407754811 ) ) ;
#18147 = CARTESIAN_POINT ( 'NONE',  ( 16.56872352241294521, 0.009207754980063749192, 0.004907101719994666836 ) ) ;
#18148 = B_SPLINE_CURVE_WITH_KNOTS ( 'NONE', 3,
 ( #17954, #9520, #3404, #10969, #5217, #13819 ),
 .UNSPECIFIED., .F., .F.,
 ( 4, 2, 4 ),
 ( 2.168404344971008868E-19, 0.0001828790815886944003, 0.0003657581631773885837 ),
 .UNSPECIFIED. ) ;
#18149 = DIRECTION ( 'NONE',  ( -1.000000000000000000, 0.000000000000000000, 0.000000000000000000 ) ) ;
#18150 = EDGE_LOOP ( 'NONE', ( #9698, #3347, #18233, #5300 ) ) ;
#18151 = CARTESIAN_POINT ( 'NONE',  ( 16.58200780006414732, 0.0006320991582349651770, -0.01115192838421568376 ) ) ;
#18152 = CARTESIAN_POINT ( 'NONE',  ( 8.522092701127531811, -5.841710761610102942, -3.777034505568587885 ) ) ;
#18153 = CARTESIAN_POINT ( 'NONE',  ( -0.6292663627301623430, 7.499999999999999112, -14.32718894987469938 ) ) ;
#18154 = FACE_OUTER_BOUND ( 'NONE', #1823, .T. ) ;
#18155 = CARTESIAN_POINT ( 'NONE',  ( 3.950837973638668288, 0.000000000000000000, 0.000000000000000000 ) ) ;
#18156 = CARTESIAN_POINT ( 'NONE',  ( 0.3151926232592466293, 13.04305446098362253, -4.318679262939488339 ) ) ;
#18157 =( BOUNDED_SURFACE ( )  B_SPLINE_SURFACE ( 3, 1, ( 
 ( #15528, #14095 ),
 ( #2614, #11426 ),
 ( #9704, #17246 ),
 ( #5573, #9980 ) ),
 .UNSPECIFIED., .F., .F., .T. ) 
 B_SPLINE_SURFACE_WITH_KNOTS ( ( 4, 4 ),
 ( 2, 2 ),
 ( 0.000000000000000000, 1.000000000000000000 ),
 ( 0.000000000000000000, 1.000000000000000000 ),
 .UNSPECIFIED. ) 
 GEOMETRIC_REPRESENTATION_ITEM ( )  RATIONAL_B_SPLINE_SURFACE ( (
 ( 1.000000000000000000, 1.000000000000000000),
 ( 0.9933953342250436691, 0.8357391271907733676),
 ( 0.9933953342250436691, 0.8357391271907733676),
 ( 1.000000000000000000, 1.000000000000000000) ) ) 
 REPRESENTATION_ITEM ( '' )  SURFACE ( )  );
#18158 =( BOUNDED_SURFACE ( )  B_SPLINE_SURFACE ( 3, 1, ( 
 ( #8897, #2859 ),
 ( #18739, #8807 ),
 ( #17214, #15969 ),
 ( #5638, #4130 ) ),
 .UNSPECIFIED., .F., .F., .T. ) 
 B_SPLINE_SURFACE_WITH_KNOTS ( ( 4, 4 ),
 ( 2, 2 ),
 ( 0.000000000000000000, 1.000000000000000000 ),
 ( 0.000000000000000000, 1.000000000000000000 ),
 .UNSPECIFIED. ) 
 GEOMETRIC_REPRESENTATION_ITEM ( )  RATIONAL_B_SPLINE_SURFACE ( (
 ( 1.000000000000000000, 1.000000000000000000),
 ( 0.9593108457356467333, 0.9995965569486454649),
 ( 0.9593108457356467333, 0.9995965569486454649),
 ( 1.000000000000000000, 1.000000000000000000) ) ) 
 REPRESENTATION_ITEM ( '' )  SURFACE ( )  );
#18159 = CIRCLE ( 'NONE', #1045, 16.06066017081991149 ) ;
#18160 = ORIENTED_EDGE ( 'NONE', *, *, #4504, .F. ) ;
#18161 = EDGE_CURVE ( 'NONE', #10527, #12010, #16327, .T. ) ;
#18162 = VECTOR ( 'NONE', #6798, 1000.000000000000000 ) ;
#18164 = ORIENTED_EDGE ( 'NONE', *, *, #5885, .T. ) ;
#18163 = CARTESIAN_POINT ( 'NONE',  ( 3.950837973638675393, 6.888253895133479965, -12.81214529934967672 ) ) ;
#18165 = CARTESIAN_POINT ( 'NONE',  ( 2.002547531651519996, 11.75462648437108015, -4.532360870844206246 ) ) ;
#18166 = AXIS2_PLACEMENT_3D ( 'NONE', #8502, #17282, #8233 ) ;
#18167 = B_SPLINE_CURVE_WITH_KNOTS ( 'NONE', 3,
 ( #5271, #8251, #12352, #792, #11025, #3745, #18188, #11115, #9399, #3842, #9671, #15228, #2398 ),
 .UNSPECIFIED., .F., .F.,
 ( 4, 3, 3, 3, 4 ),
 ( 4.906538933386797396E-18, 0.0002299780670421066068, 0.0004599561239687925598, 0.0006896788984287864372, 0.0009194956271626387621 ),
 .UNSPECIFIED. ) ;
#18168 = EDGE_CURVE ( 'NONE', #9580, #12603, #1150, .T. ) ;
#18169 = VERTEX_POINT ( 'NONE', #12712 ) ;
#18170 = CARTESIAN_POINT ( 'NONE',  ( 2.002547531651519996, -4.532360870844247991, -11.75462648437106417 ) ) ;
#18171 = CARTESIAN_POINT ( 'NONE',  ( -0.7597029211758296041, -7.500000000000000888, -14.39758526244282599 ) ) ;
#18172 = EDGE_LOOP ( 'NONE', ( #18231, #1063, #15853, #2720 ) ) ;
#18173 = CARTESIAN_POINT ( 'NONE',  ( 1.254255976357671720, -9.426444230097072108, 11.25336128106933664 ) ) ;
#18174 = CARTESIAN_POINT ( 'NONE',  ( 8.438534575730034959, -5.688336279099016402, -3.845978796786099885 ) ) ;
#18175 = AXIS2_PLACEMENT_3D ( 'NONE', #17713, #7682, #7590 ) ;
#18176 = FACE_OUTER_BOUND ( 'NONE', #18011, .T. ) ;
#18177 = CIRCLE ( 'NONE', #13279, 14.54644660717763927 ) ;
#18178 = DIRECTION ( 'NONE',  ( 0.000000000000000000, -1.000000000000000000, 0.000000000000000000 ) ) ;
#18179 = EDGE_CURVE ( 'NONE', #13361, #2604, #15764, .T. ) ;
#18180 = CARTESIAN_POINT ( 'NONE',  ( 1.846138399168762989, -3.446241763653083101, 11.95493567637849530 ) ) ;
#18181 = EDGE_CURVE ( 'NONE', #13031, #8021, #6568, .T. ) ;
#18182 = EDGE_CURVE ( 'NONE', #11277, #8048, #9002, .T. ) ;
#18183 = CARTESIAN_POINT ( 'NONE',  ( 0.4754618798421162973, -10.80499583390518836, 8.775436892861078420 ) ) ;
#18185 = ORIENTED_EDGE ( 'NONE', *, *, #2382, .T. ) ;
#18184 = CARTESIAN_POINT ( 'NONE',  ( 1.861628059977342042, 10.38573835516722355, -6.879051339207178373 ) ) ;
#18186 = DIRECTION ( 'NONE',  ( -1.000000000000000000, -0.000000000000000000, -0.000000000000000000 ) ) ;
#18187 = VERTEX_POINT ( 'NONE', #12897 ) ;
#18188 = CARTESIAN_POINT ( 'NONE',  ( 0.3151928476913571364, -11.11539186930580669, -8.075547435847068911 ) ) ;
#18189 = FACE_OUTER_BOUND ( 'NONE', #10009, .T. ) ;
#18190 = EDGE_LOOP ( 'NONE', ( #1203, #11843, #10180, #17547 ) ) ;
#18191 = ORIENTED_EDGE ( 'NONE', *, *, #4468, .T. ) ;
#18192 = PLANE ( 'NONE',  #9419 ) ;
#18193 = DIRECTION ( 'NONE',  ( 0.000000000000000000, -0.000000000000000000, -1.000000000000000000 ) ) ;
#18194 = ORIENTED_EDGE ( 'NONE', *, *, #951, .F. ) ;
#18195 = EDGE_CURVE ( 'NONE', #8066, #5247, #8415, .T. ) ;
#18196 = PRESENTATION_STYLE_ASSIGNMENT (( #7704 ) ) ;
#18197 = DIRECTION ( 'NONE',  ( -0.000000000000000000, 0.000000000000000000, 1.000000000000000000 ) ) ;
#18198 = DIRECTION ( 'NONE',  ( 0.7561779333270775005, -0.4122479608995778255, 0.5081796452863200919 ) ) ;
#18199 = CARTESIAN_POINT ( 'NONE',  ( 5.000000000000000000, 0.000000000000000000, -3.000000000000000000 ) ) ;
#18200 = FACE_BOUND ( 'NONE', #3120, .T. ) ;
#18201 = SHAPE_DEFINITION_REPRESENTATION ( #13324, #11674 ) ;
#18202 = FILL_AREA_STYLE ('',( #3382 ) ) ;
#18203 = CARTESIAN_POINT ( 'NONE',  ( 1.846138399168762101, 10.30487220521580305, -6.971848976710897539 ) ) ;
#18204 = LINE ( 'NONE', #13894, #5713 ) ;
#18205 = ORIENTED_EDGE ( 'NONE', *, *, #18133, .F. ) ;
#18206 = CARTESIAN_POINT ( 'NONE',  ( 0.3720661004400040439, -12.89739157014196635, 4.951033743989591507 ) ) ;
#18207 = CARTESIAN_POINT ( 'NONE',  ( 1.977436885026099711, -15.33079650480437550, -1.488549889122204650 ) ) ;
#18208 = CARTESIAN_POINT ( 'NONE',  ( 0.3307726912345229087, -13.25328329128663007, -3.680742887039447631 ) ) ;
#18209 = CARTESIAN_POINT ( 'NONE',  ( 0.000000000000000000, 0.8660254037844389297, -1.500000000000000000 ) ) ;
#18210 = EDGE_LOOP ( 'NONE', ( #7257, #7428, #4887, #15114 ) ) ;
#18211 = EDGE_CURVE ( 'NONE', #10910, #15874, #12806, .T. ) ;
#18212 = ORIENTED_EDGE ( 'NONE', *, *, #12490, .F. ) ;
#18213 = ORIENTED_EDGE ( 'NONE', *, *, #1779, .T. ) ;
#18214 = STYLED_ITEM ( 'NONE', ( #16652 ), #18307 ) ;
#18215 = VERTEX_POINT ( 'NONE', #5532 ) ;
#18216 = CIRCLE ( 'NONE', #11817, 4.999999999999997335 ) ;
#18217 = ADVANCED_FACE ( 'NONE', ( #17291 ), #2752, .T. ) ;
#18218 = DIRECTION ( 'NONE',  ( -1.913297951445007622E-16, 1.000000000000000000, 0.000000000000000000 ) ) ;
#18219 = CARTESIAN_POINT ( 'NONE',  ( -5.322906077793310153, -7.500000000000001776, -16.88078391064166439 ) ) ;
#18220 = B_SPLINE_CURVE_WITH_KNOTS ( 'NONE', 3,
 ( #6452, #2411, #8172, #3479, #894, #3575 ),
 .UNSPECIFIED., .F., .F.,
 ( 4, 2, 4 ),
 ( 0.000000000000000000, 0.0001828790815886942919, 0.0003657581631773885837 ),
 .UNSPECIFIED. ) ;
#18221 = AXIS2_PLACEMENT_3D ( 'NONE', #6321, #13678, #13850 ) ;
#18222 = ORIENTED_EDGE ( 'NONE', *, *, #14759, .T. ) ;
#18223 = CARTESIAN_POINT ( 'NONE',  ( 1.846138399168762101, -9.815003036200465658, 7.646096044339859787 ) ) ;
#18224 = CARTESIAN_POINT ( 'NONE',  ( 2.636624412715137922, -7.605649742761668719, 14.14563173255331741 ) ) ;
#18225 = VECTOR ( 'NONE', #12647, 1000.000000000000000 ) ;
#18226 = TOROIDAL_SURFACE ( 'NONE', #1745, 2.700000000000000178, 0.2000000000000000111 ) ;
#18227 = CARTESIAN_POINT ( 'NONE',  ( 0.4754618798421171855, -3.583352865732766901, 13.45049478164058598 ) ) ;
#18228 = DIRECTION ( 'NONE',  ( 0.000000000000000000, 0.000000000000000000, 1.000000000000000000 ) ) ;
#18229 = DIRECTION ( 'NONE',  ( 0.000000000000000000, -1.000000000000000000, 0.000000000000000000 ) ) ;
#18230 = CARTESIAN_POINT ( 'NONE',  ( -5.000000000000000888, 17.00000000000000000, 4.000000000000000000 ) ) ;
#18231 = ORIENTED_EDGE ( 'NONE', *, *, #351, .F. ) ;
#18232 =( BOUNDED_SURFACE ( )  B_SPLINE_SURFACE ( 3, 1, ( 
 ( #17716, #11503 ),
 ( #4416, #8815 ),
 ( #17613, #17321 ),
 ( #14451, #4616 ) ),
 .UNSPECIFIED., .F., .F., .T. ) 
 B_SPLINE_SURFACE_WITH_KNOTS ( ( 4, 4 ),
 ( 2, 2 ),
 ( 0.000000000000000000, 1.000000000000000000 ),
 ( 0.000000000000000000, 1.000000000000000000 ),
 .UNSPECIFIED. ) 
 GEOMETRIC_REPRESENTATION_ITEM ( )  RATIONAL_B_SPLINE_SURFACE ( (
 ( 1.000000000000000000, 1.000000000000000000),
 ( 0.9933953342250436691, 0.8357391271907733676),
 ( 0.9933953342250436691, 0.8357391271907733676),
 ( 1.000000000000000000, 1.000000000000000000) ) ) 
 REPRESENTATION_ITEM ( '' )  SURFACE ( )  );
#18233 = ORIENTED_EDGE ( 'NONE', *, *, #1262, .T. ) ;
#18234 = ORIENTED_EDGE ( 'NONE', *, *, #16867, .T. ) ;
#18235 = EDGE_LOOP ( 'NONE', ( #17100, #1223, #14156, #5562 ) ) ;
#18236 = CARTESIAN_POINT ( 'NONE',  ( 0.3720661004400037664, -13.79610186261029270, -0.7231997263366251039 ) ) ;
#18237 = CIRCLE ( 'NONE', #13351, 1.500000000000000000 ) ;
#18238 = EDGE_CURVE ( 'NONE', #11022, #13051, #10353, .T. ) ;
#18239 = EDGE_CURVE ( 'NONE', #1814, #202, #5340, .T. ) ;
#18240 = EDGE_CURVE ( 'NONE', #10527, #12474, #10619, .T. ) ;
#18241 = CARTESIAN_POINT ( 'NONE',  ( 1.104287921197080512E-14, -9.013167318348349610, 25.01316734529528674 ) ) ;
#18242 = CARTESIAN_POINT ( 'NONE',  ( 3.074695600507125981, -2.772091048739183439, -15.30693405987811673 ) ) ;
#18243 = CARTESIAN_POINT ( 'NONE',  ( 2.353870697619111496, -4.720869121224215093, 12.05847592522641953 ) ) ;
#18244 = CARTESIAN_POINT ( 'NONE',  ( 3.950837973638668288, 0.000000000000000000, 0.000000000000000000 ) ) ;
#18245 = ORIENTED_EDGE ( 'NONE', *, *, #801, .F. ) ;
#18246 = CARTESIAN_POINT ( 'NONE',  ( 16.56753206892534891, -0.001421777558676013808, 0.009389754735542241854 ) ) ;
#18247 = CARTESIAN_POINT ( 'NONE',  ( 1.847412631396500693, -11.82061107079961992, -3.886120457021520647 ) ) ;
#18248 = B_SPLINE_CURVE_WITH_KNOTS ( 'NONE', 3,
 ( #2282, #944, #6599, #12423, #5337, #12073 ),
 .UNSPECIFIED., .F., .F.,
 ( 4, 2, 4 ),
 ( 0.000000000000000000, 0.001656992708823338926, 0.003313985417646677853 ),
 .UNSPECIFIED. ) ;
#18249 = CARTESIAN_POINT ( 'NONE',  ( -2.576507258268692535, 7.499999999999999112, -13.18245040793292233 ) ) ;
#18250 = DIRECTION ( 'NONE',  ( 0.000000000000000000, 0.000000000000000000, 1.000000000000000000 ) ) ;
#18251 = DIRECTION ( 'NONE',  ( 0.000000000000000000, 0.000000000000000000, -1.000000000000000000 ) ) ;
#18252 = FACE_OUTER_BOUND ( 'NONE', #2669, .T. ) ;
#18253 = CARTESIAN_POINT ( 'NONE',  ( -66.35602477868047799, 0.000000000000000000, -2.000000000000000000 ) ) ;
#18254 = CARTESIAN_POINT ( 'NONE',  ( -32.49999999999999289, -12.50000000000000178, 3.000000000000000000 ) ) ;
#18255 = ORIENTED_EDGE ( 'NONE', *, *, #6047, .T. ) ;
#18257 = VERTEX_POINT ( 'NONE', #17977 ) ;
#18256 = PLANE ( 'NONE',  #17919 ) ;
#18258 = CARTESIAN_POINT ( 'NONE',  ( 0.4384471787762814765, 4.978024343489044767, 12.93784327393174571 ) ) ;
#18259 = VECTOR ( 'NONE', #15935, 1000.000000000000114 ) ;
#18260 = EDGE_LOOP ( 'NONE', ( #10771, #9914, #2764, #13057, #16533 ) ) ;
#18261 = CARTESIAN_POINT ( 'NONE',  ( 1.846138399168762101, -3.446241763652916124, -11.95493567637853971 ) ) ;
#18262 = CARTESIAN_POINT ( 'NONE',  ( -5.275788075193909243, -7.500000000000000888, -12.98022329939712094 ) ) ;
#18263 = EDGE_CURVE ( 'NONE', #1860, #349, #6026, .T. ) ;
#18264 = ORIENTED_EDGE ( 'NONE', *, *, #491, .F. ) ;
#18265 = DIRECTION ( 'NONE',  ( 1.000000000000000000, -0.000000000000000000, -0.000000000000000000 ) ) ;
#18266 = FACE_OUTER_BOUND ( 'NONE', #5541, .T. ) ;
#18267 = EDGE_CURVE ( 'NONE', #1614, #4817, #3056, .T. ) ;
#18268 = DIRECTION ( 'NONE',  ( -1.000000000000000000, -0.000000000000000000, -0.000000000000000000 ) ) ;
#18269 =( BOUNDED_SURFACE ( )  B_SPLINE_SURFACE ( 3, 1, ( 
 ( #6683, #16805 ),
 ( #2272, #18326 ),
 ( #18058, #5323 ),
 ( #15277, #9628 ) ),
 .UNSPECIFIED., .F., .F., .T. ) 
 B_SPLINE_SURFACE_WITH_KNOTS ( ( 4, 4 ),
 ( 2, 2 ),
 ( 0.000000000000000000, 1.000000000000000000 ),
 ( 0.000000000000000000, 1.000000000000000000 ),
 .UNSPECIFIED. ) 
 GEOMETRIC_REPRESENTATION_ITEM ( )  RATIONAL_B_SPLINE_SURFACE ( (
 ( 1.000000000000000000, 1.000000000000000000),
 ( 0.9593108457356467333, 0.9995965569486454649),
 ( 0.9593108457356467333, 0.9995965569486454649),
 ( 1.000000000000000000, 1.000000000000000000) ) ) 
 REPRESENTATION_ITEM ( '' )  SURFACE ( )  );
#18270 = DIRECTION ( 'NONE',  ( -1.000000000000000000, -0.000000000000000000, -0.000000000000000000 ) ) ;
#18271 = CIRCLE ( 'NONE', #11855, 2.500000000000000888 ) ;
#18272 =( NAMED_UNIT ( * ) PLANE_ANGLE_UNIT ( ) SI_UNIT ( $, .RADIAN. ) );
#18273 = CARTESIAN_POINT ( 'NONE',  ( 2.320521194584054037, 7.743190876765937425, -13.71278319228217946 ) ) ;
#18274 = FACE_OUTER_BOUND ( 'NONE', #5804, .T. ) ;
#18276 = ORIENTED_EDGE ( 'NONE', *, *, #1816, .F. ) ;
#18275 = CARTESIAN_POINT ( 'NONE',  ( 0.3058872367615230181, -0.6080468242579999405, -13.72992299905060776 ) ) ;
#18277 = CARTESIAN_POINT ( 'NONE',  ( 0.4754618798421171855, -5.007009103465158262, -12.98792082933649716 ) ) ;
#18278 = B_SPLINE_CURVE_WITH_KNOTS ( 'NONE', 3,
 ( #15743, #15934, #17177, #15841, #14121, #15558 ),
 .UNSPECIFIED., .F., .F.,
 ( 4, 2, 4 ),
 ( 4.005364051932256883E-17, 0.0002014099069817290285, 0.0004028198139634179956 ),
 .UNSPECIFIED. ) ;
#18279 = CARTESIAN_POINT ( 'NONE',  ( 0.3137051932979792457, -13.73004976592202375, 0.4596302728639276580 ) ) ;
#18280 = CARTESIAN_POINT ( 'NONE',  ( 0.4754618798421171855, -0.7484603771383426807, -13.89949764182683545 ) ) ;
#18281 = DIRECTION ( 'NONE',  ( 1.000000000000000000, 2.891205793294679805E-16, 0.000000000000000000 ) ) ;
#18282 = EDGE_LOOP ( 'NONE', ( #17787, #12978, #10604, #13453 ) ) ;
#18283 = ORIENTED_EDGE ( 'NONE', *, *, #12187, .T. ) ;
#18284 = DIRECTION ( 'NONE',  ( 0.7635533937278214944, -0.6071939193889578368, -0.2197766120036483140 ) ) ;
#18285 = DIRECTION ( 'NONE',  ( -1.000000000000000000, -0.000000000000000000, -0.000000000000000000 ) ) ;
#18286 = ORIENTED_EDGE ( 'NONE', *, *, #3323, .F. ) ;
#18287 = CARTESIAN_POINT ( 'NONE',  ( 0.3148213771069390265, 4.026433757158980775, 13.13560149728601978 ) ) ;
#18288 = CARTESIAN_POINT ( 'NONE',  ( 16.57778382496167424, 0.01482878558584695486, -0.001819584982831739346 ) ) ;
#18289 = ADVANCED_FACE ( 'NONE', ( #7757 ), #1721, .F. ) ;
#18290 = CARTESIAN_POINT ( 'NONE',  ( 0.4754618798421162973, -11.68486377711971969, 7.564402563418428649 ) ) ;
#18291 = PLANE ( 'NONE',  #6872 ) ;
#18292 = LINE ( 'NONE', #15325, #12419 ) ;
#18293 = CARTESIAN_POINT ( 'NONE',  ( 25.00000000000000000, -7.500000000000000888, -17.00000000000000000 ) ) ;
#18294 = APPLICATION_PROTOCOL_DEFINITION ( 'draft international standard', 'automotive_design', 1998, #14862 ) ;
#18295 = CARTESIAN_POINT ( 'NONE',  ( 0.3151928476913565258, -13.06671852871092199, 4.245853234426333778 ) ) ;
#18296 = CARTESIAN_POINT ( 'NONE',  ( 0.3095370825347233956, -12.91933430393611104, 4.681152801286112997 ) ) ;
#18297 = CARTESIAN_POINT ( 'NONE',  ( 0.3137051932979775248, -12.91601973349273891, 4.679953077377436266 ) ) ;
#18298 = ADVANCED_FACE ( 'NONE', ( #3431 ), #3115, .F. ) ;
#18299 = AXIS2_PLACEMENT_3D ( 'NONE', #14698, #17575, #3222 ) ;
#18300 = DIRECTION ( 'NONE',  ( 0.7561779333270775005, 0.3559159372837274460, 0.5491072561318377510 ) ) ;
#18301 = CARTESIAN_POINT ( 'NONE',  ( 8.438534575730034959, 5.415535776177581972, -4.221456476902606170 ) ) ;
#18302 = VECTOR ( 'NONE', #3008, 1000.000000000000114 ) ;
#18303 = ORIENTED_EDGE ( 'NONE', *, *, #14386, .T. ) ;
#18304 = VERTEX_POINT ( 'NONE', #4686 ) ;
#18305 = ORIENTED_EDGE ( 'NONE', *, *, #1659, .F. ) ;
#18306 = VERTEX_POINT ( 'NONE', #17587 ) ;
#18307 = ADVANCED_BREP_SHAPE_REPRESENTATION ( '', ( #16636, #2030 ), #16378 ) ;
#18308 = CARTESIAN_POINT ( 'NONE',  ( 1.500000000000000000, 2.869946927167511679E-16, 7.000000000000000000 ) ) ;
#18309 = CARTESIAN_POINT ( 'NONE',  ( -1.333872087798559480, -7.500000000000001776, -14.76174338479138726 ) ) ;
#18310 = CARTESIAN_POINT ( 'NONE',  ( 1.918921323896323639, -3.258415356426438869, -12.08297777410668417 ) ) ;
#18311 = CARTESIAN_POINT ( 'NONE',  ( 0.4862570985993235340, -7.559321496869506163, 11.67702470553362559 ) ) ;
#18312 = EDGE_CURVE ( 'NONE', #6301, #10648, #7809, .T. ) ;
#18313 = CARTESIAN_POINT ( 'NONE',  ( 2.747332970342022840, 11.66639548242823921, -11.45495994260705075 ) ) ;
#18314 = CARTESIAN_POINT ( 'NONE',  ( 3.074695600508143833, 13.70113613813285269, 7.366518011945069055 ) ) ;
#18315 = CARTESIAN_POINT ( 'NONE',  ( 2.002547531651519996, -7.942910686618240845, 9.778737580845669797 ) ) ;
#18316 = CARTESIAN_POINT ( 'NONE',  ( 16.56679352167444819, 0.001390132774595458174, 0.009190982326619367287 ) ) ;
#18317 = CARTESIAN_POINT ( 'NONE',  ( 16.56822296793089322, 0.002414375228568836022, 0.009847136207495320662 ) ) ;
#18318 = EDGE_LOOP ( 'NONE', ( #12080, #7985, #6673, #10090, #11911, #4628 ) ) ;
#18319 = ORIENTED_EDGE ( 'NONE', *, *, #13944, .T. ) ;
#18320 = EDGE_LOOP ( 'NONE', ( #7430, #4553, #2359, #746, #8718, #11861 ) ) ;
#18321 = VERTEX_POINT ( 'NONE', #9174 ) ;
#18322 = LINE ( 'NONE', #2700, #693 ) ;
#18323 = CIRCLE ( 'NONE', #326, 16.06066017081991149 ) ;
#18324 = CARTESIAN_POINT ( 'NONE',  ( 16.56872352241294521, -0.001442253899401298341, 0.01033355228142499027 ) ) ;
#18325 = CARTESIAN_POINT ( 'NONE',  ( 2.002547531651519996, 12.17374746633582561, -3.242439124566524278 ) ) ;
#18326 = CARTESIAN_POINT ( 'NONE',  ( 0.3170788640506441158, -13.74111462631963576, 0.1533108587035682813 ) ) ;
#18327 = CARTESIAN_POINT ( 'NONE',  ( 0.4384471787762835859, 13.39294437382618419, 3.577367180593594043 ) ) ;
#18328 = ORIENTED_EDGE ( 'NONE', *, *, #18440, .F. ) ;
#18329 = CARTESIAN_POINT ( 'NONE',  ( 0.3720661004400040439, -8.694226082900513575, -10.73619472937711983 ) ) ;
#18330 = CARTESIAN_POINT ( 'NONE',  ( 1.918918678667072886, 0.6348738215465219437, 12.49849921341423453 ) ) ;
#18331 = B_SPLINE_CURVE_WITH_KNOTS ( 'NONE', 3,
 ( #16427, #7439, #13540, #9151, #267, #14974, #17667, #13355, #1896, #13448, #7731, #11829, #16225 ),
 .UNSPECIFIED., .F., .F.,
 ( 4, 3, 3, 3, 4 ),
 ( 3.127317220692750759E-18, 0.0002299780670421087210, 0.0004599561239687931019, 0.0006896788984287912077, 0.0009194956271626412558 ),
 .UNSPECIFIED. ) ;
#18332 = CARTESIAN_POINT ( 'NONE',  ( -2.953963787679199537, 6.378445150919402451, -12.00000001548991158 ) ) ;
#18333 = CARTESIAN_POINT ( 'NONE',  ( 0.000000000000000000, 1.732050807568878747, 7.017607234860990640E-28 ) ) ;
#18334 = CARTESIAN_POINT ( 'NONE',  ( -1.389456752619696367, -44.31487138727242581, 6.000000000000000000 ) ) ;
#18335 = DIRECTION ( 'NONE',  ( 1.000000000000000000, 0.000000000000000000, 0.000000000000000000 ) ) ;
#18336 = CARTESIAN_POINT ( 'NONE',  ( 0.3151928479966099039, 0.07658992383256929548, -13.73922861026898623 ) ) ;
#18337 =( BOUNDED_SURFACE ( )  B_SPLINE_SURFACE ( 3, 1, ( 
 ( #2258, #4949 ),
 ( #4858, #2092 ),
 ( #3605, #832 ),
 ( #737, #8105 ) ),
 .UNSPECIFIED., .F., .F., .T. ) 
 B_SPLINE_SURFACE_WITH_KNOTS ( ( 4, 4 ),
 ( 2, 2 ),
 ( 0.000000000000000000, 1.000000000000000000 ),
 ( 0.000000000000000000, 1.000000000000000000 ),
 .UNSPECIFIED. ) 
 GEOMETRIC_REPRESENTATION_ITEM ( )  RATIONAL_B_SPLINE_SURFACE ( (
 ( 1.000000000000000000, 1.000000000000000000),
 ( 0.9933953342250438912, 0.8357391271907739227),
 ( 0.9933953342250438912, 0.8357391271907739227),
 ( 1.000000000000000000, 1.000000000000000000) ) ) 
 REPRESENTATION_ITEM ( '' )  SURFACE ( )  );
#18338 = EDGE_CURVE ( 'NONE', #8143, #8310, #1686, .T. ) ;
#18339 = CARTESIAN_POINT ( 'NONE',  ( 2.353870697619111496, 12.53036919722789477, -3.268530966681500782 ) ) ;
#18340 = ADVANCED_FACE ( 'NONE', ( #14999 ), #2004, .T. ) ;
#18341 = ORIENTED_EDGE ( 'NONE', *, *, #13748, .T. ) ;
#18342 = B_SPLINE_CURVE_WITH_KNOTS ( 'NONE', 3,
 ( #362, #9152, #1695, #17856, #1598, #11733, #6189, #16227, #5994, #8956, #14782, #463, #7442 ),
 .UNSPECIFIED., .F., .F.,
 ( 4, 3, 3, 3, 4 ),
 ( 1.734723475976806902E-18, 0.0002299804304191488261, 0.0004599608082120263644, 0.0006467586077648019086, 0.0008336169836826000249 ),
 .UNSPECIFIED. ) ;
#18344 = ORIENTED_EDGE ( 'NONE', *, *, #10868, .T. ) ;
#18343 = DIRECTION ( 'NONE',  ( -0.000000000000000000, 1.000000000000000000, -0.000000000000000000 ) ) ;
#18345 = CARTESIAN_POINT ( 'NONE',  ( 0.000000000000000000, 0.000000000000000000, 5.000000000000000000 ) ) ;
#18346 = VECTOR ( 'NONE', #7828, 1000.000000000000000 ) ;
#18347 = CARTESIAN_POINT ( 'NONE',  ( 1.847426409206450959, -2.029922383240494730E-11, 12.44303504652081038 ) ) ;
#18348 = EDGE_LOOP ( 'NONE', ( #3600, #17376, #11028, #8681 ) ) ;
#18349 = CARTESIAN_POINT ( 'NONE',  ( 2.002547531651519996, 4.532360870844494016, -11.75462648437097180 ) ) ;
#18350 = DIRECTION ( 'NONE',  ( 0.000000000000000000, 0.000000000000000000, -1.000000000000000000 ) ) ;
#18351 = ORIENTED_EDGE ( 'NONE', *, *, #17099, .F. ) ;
#18352 = CARTESIAN_POINT ( 'NONE',  ( 3.664313757352975376, 9.645155442698909454, -10.50730552161222597 ) ) ;
#18353 = CARTESIAN_POINT ( 'NONE',  ( 0.3939822652208125331, -13.34132036472939831, 3.598529276937210142 ) ) ;
#18354 = CARTESIAN_POINT ( 'NONE',  ( 0.000000000000000000, 0.000000000000000000, -13.00000000000000533 ) ) ;
#18355 = CARTESIAN_POINT ( 'NONE',  ( -26.50000000000000711, -12.50000000000000178, -1.000000000000000000 ) ) ;
#18356 = CARTESIAN_POINT ( 'NONE',  ( 0.3151928479966097929, -0.07658992383253612757, 13.73922861026898623 ) ) ;
#18357 = B_SPLINE_CURVE_WITH_KNOTS ( 'NONE', 3,
 ( #593, #4974, #494, #18163 ),
 .UNSPECIFIED., .F., .F.,
 ( 4, 4 ),
 ( 4.589925559575316169E-16, 0.002004993803842821786 ),
 .UNSPECIFIED. ) ;
#18358 = CIRCLE ( 'NONE', #7698, 12.15840553252917289 ) ;
#18359 = EDGE_CURVE ( 'NONE', #4248, #12932, #16354, .T. ) ;
#18360 = CARTESIAN_POINT ( 'NONE',  ( 2.636624412716062960, 2.862162146982868194, -15.80357026013419564 ) ) ;
#18361 = EDGE_CURVE ( 'NONE', #8605, #17143, #11045, .T. ) ;
#18362 = FACE_OUTER_BOUND ( 'NONE', #16336, .T. ) ;
#18364 = ORIENTED_EDGE ( 'NONE', *, *, #4338, .T. ) ;
#18363 = DIRECTION ( 'NONE',  ( -1.000000000000000000, -0.000000000000000000, -0.000000000000000000 ) ) ;
#18365 = LINE ( 'NONE', #5179, #4501 ) ;
#18366 = CARTESIAN_POINT ( 'NONE',  ( 0.4384471787762829753, 8.732395932355681012, 10.76632603192789617 ) ) ;
#18367 = CARTESIAN_POINT ( 'NONE',  ( 0.3150686449036048664, -4.391272911157235725, -13.01866258978841628 ) ) ;
#18368 = EDGE_LOOP ( 'NONE', ( #958, #11423, #6198, #2080 ) ) ;
#18369 = ORIENTED_EDGE ( 'NONE', *, *, #17124, .F. ) ;
#18370 = CARTESIAN_POINT ( 'NONE',  ( 22.30499999999999972, 0.000000000000000000, 0.000000000000000000 ) ) ;
#18371 = CARTESIAN_POINT ( 'NONE',  ( 2.002547531651519996, -6.845637710436110801, -10.57595306287299763 ) ) ;
#18372 = EDGE_LOOP ( 'NONE', ( #8472, #16181 ) ) ;
#18373 = CARTESIAN_POINT ( 'NONE',  ( 0.3151930723728439410, 4.172946285306569969, 13.09040889075571990 ) ) ;
#18374 = DIRECTION ( 'NONE',  ( -0.000000000000000000, 0.5000000000000004441, 0.8660254037844383745 ) ) ;
#18375 =( NAMED_UNIT ( * ) PLANE_ANGLE_UNIT ( ) SI_UNIT ( $, .RADIAN. ) );
#18376 = AXIS2_PLACEMENT_3D ( 'NONE', #14915, #13103, #8802 ) ;
#18377 = DIRECTION ( 'NONE',  ( 0.4246593920385850485, 0.1376957914266804250, -0.8948208031649687033 ) ) ;
#18378 = B_SPLINE_CURVE_WITH_KNOTS ( 'NONE', 3,
 ( #16494, #9219, #538, #18445 ),
 .UNSPECIFIED., .F., .F.,
 ( 4, 4 ),
 ( 0.000000000000000000, 0.002004993803842688646 ),
 .UNSPECIFIED. ) ;
#18379 = CARTESIAN_POINT ( 'NONE',  ( 3.074695600507272086, 15.41438262616223298, -2.093687500612007923 ) ) ;
#18380 = CARTESIAN_POINT ( 'NONE',  ( 1.846138399168762101, 7.646096044339892650, 9.815003036200437236 ) ) ;
#18381 = APPLICATION_PROTOCOL_DEFINITION ( 'draft international standard', 'automotive_design', 1998, #17804 ) ;
#18382 = CARTESIAN_POINT ( 'NONE',  ( -194.9999999999999716, -10.00000000000002665, 6.000000000000000000 ) ) ;
#18383 = DIRECTION ( 'NONE',  ( -0.000000000000000000, -0.000000000000000000, 1.000000000000000000 ) ) ;
#18384 = CARTESIAN_POINT ( 'NONE',  ( -5.000000000000000888, 17.00000000000000000, 4.000000000000000000 ) ) ;
#18385 = DIRECTION ( 'NONE',  ( -0.000000000000000000, -0.000000000000000000, 1.000000000000000000 ) ) ;
#18386 = EDGE_CURVE ( 'NONE', #17057, #12585, #9449, .T. ) ;
#18387 = DIRECTION ( 'NONE',  ( -0.000000000000000000, 1.000000000000000000, -0.000000000000000000 ) ) ;
#18388 = EDGE_LOOP ( 'NONE', ( #14575, #9854, #10228, #34 ) ) ;
#18389 = ORIENTED_EDGE ( 'NONE', *, *, #15651, .F. ) ;
#18390 = B_SPLINE_CURVE_WITH_KNOTS ( 'NONE', 3,
 ( #18347, #15751, #7068, #11283, #16823, #15652, #12882, #5161, #3726, #2291 ),
 .UNSPECIFIED., .F., .F.,
 ( 4, 3, 3, 4 ),
 ( 0.0004168119862255878537, 0.0004599608082120251176, 0.0006467586077648016917, 0.0008336169836825990491 ),
 .UNSPECIFIED. ) ;
#18391 = ORIENTED_EDGE ( 'NONE', *, *, #16392, .F. ) ;
#18392 = ORIENTED_EDGE ( 'NONE', *, *, #2443, .F. ) ;
#18393 = CIRCLE ( 'NONE', #7427, 10.00000000000000888 ) ;
#18394 = LINE ( 'NONE', #642, #8721 ) ;
#18395 = LINE ( 'NONE', #11147, #5319 ) ;
#18396 = LINE ( 'NONE', #14008, #15714 ) ;
#18397 = CYLINDRICAL_SURFACE ( 'NONE', #4764, 7.000000000000000000 ) ;
#18398 = CARTESIAN_POINT ( 'NONE',  ( 0.3095370825347224519, 13.73357284481724783, -0.4597470195090672673 ) ) ;
#18399 = CARTESIAN_POINT ( 'NONE',  ( 2.123976203522053297, -6.261444813538658671, 14.31368049382967556 ) ) ;
#18400 = PRODUCT_RELATED_PRODUCT_CATEGORY ( 'part', '', ( #11962 ) ) ;
#18401 = EDGE_CURVE ( 'NONE', #8377, #3637, #193, .T. ) ;
#18402 = FACE_OUTER_BOUND ( 'NONE', #7219, .T. ) ;
#18403 = CARTESIAN_POINT ( 'NONE',  ( 16.56872352241294521, 0.004907101719994633009, -0.009207754980063766539 ) ) ;
#18404 = CIRCLE ( 'NONE', #426, 14.54644660717763927 ) ;
#18405 = VERTEX_POINT ( 'NONE', #9368 ) ;
#18406 = ADVANCED_FACE ( 'NONE', ( #16903 ), #13845, .T. ) ;
#18407 = VERTEX_POINT ( 'NONE', #8219 ) ;
#18408 = VERTEX_POINT ( 'NONE', #18334 ) ;
#18409 = EDGE_LOOP ( 'NONE', ( #12223, #15623, #2718, #2591, #6603 ) ) ;
#18410 = PLANE ( 'NONE',  #10226 ) ;
#18411 = CARTESIAN_POINT ( 'NONE',  ( 1.321128355694181398E-14, -7.013167318348350499, 16.24521815286417237 ) ) ;
#18412 = CARTESIAN_POINT ( 'NONE',  ( 3.664313757352976264, 1.627055439596472475, -14.16986885736090329 ) ) ;
#18413 = CARTESIAN_POINT ( 'NONE',  ( 1.847168016377985333, -7.161712042621529939, 10.17509564929255994 ) ) ;
#18414 = ORIENTED_EDGE ( 'NONE', *, *, #13374, .F. ) ;
#18415 = CARTESIAN_POINT ( 'NONE',  ( 0.3058872367615226295, 8.562166468153870724, -10.75034008168906396 ) ) ;
#18416 = CIRCLE ( 'NONE', #1321, 0.2000000000000000944 ) ;
#18417 = ADVANCED_FACE ( 'NONE', ( #940 ), #7676, .F. ) ;
#18418 = FACE_OUTER_BOUND ( 'NONE', #13812, .T. ) ;
#18419 = CARTESIAN_POINT ( 'NONE',  ( 1.329112640582405191, 6.875529660588472147, -12.00000000371739439 ) ) ;
#18420 = FACE_OUTER_BOUND ( 'NONE', #101, .T. ) ;
#18421 = CARTESIAN_POINT ( 'NONE',  ( -30.00000000000000355, -12.50000000000000178, 3.000000000000000000 ) ) ;
#18422 = DIRECTION ( 'NONE',  ( 0.000000000000000000, 0.000000000000000000, 1.000000000000000000 ) ) ;
#18423 = CARTESIAN_POINT ( 'NONE',  ( -12.00000000000000178, 1.469576158976824144E-15, 10.49999999999999822 ) ) ;
#18424 = DIRECTION ( 'NONE',  ( 0.000000000000000000, 0.000000000000000000, 1.000000000000000000 ) ) ;
#18425 = EDGE_LOOP ( 'NONE', ( #18160, #14909, #2379, #14574 ) ) ;
#18427 = ORIENTED_EDGE ( 'NONE', *, *, #17630, .F. ) ;
#18426 = CARTESIAN_POINT ( 'NONE',  ( 2.123976203522053741, -10.37815841598482969, -11.67822624909937090 ) ) ;
#18428 = CARTESIAN_POINT ( 'NONE',  ( 0.3720661004400040439, 8.694226082900595287, 10.73619472937705233 ) ) ;
#18429 = CIRCLE ( 'NONE', #10193, 16.06066017081991149 ) ;
#18430 = VECTOR ( 'NONE', #14783, 1000.000000000000000 ) ;
#18431 = SPHERICAL_SURFACE ( 'NONE', #8902, 5.315148208181397216 ) ;
#18432 = CARTESIAN_POINT ( 'NONE',  ( 1.560000000000000053, 0.8660254037844389297, 1.500000000000000000 ) ) ;
#18433 = EDGE_LOOP ( 'NONE', ( #15106, #8706 ) ) ;
#18434 = CARTESIAN_POINT ( 'NONE',  ( 1.918918678667044686, -4.466049546133833203, -11.69059232068582865 ) ) ;
#18435 = CARTESIAN_POINT ( 'NONE',  ( 8.438534575730034959, 2.341351102130369011, -6.454982381540262715 ) ) ;
#18436 = CARTESIAN_POINT ( 'NONE',  ( 8.438534575730034959, 6.454982381540319558, -2.341351102130211359 ) ) ;
#18437 = VERTEX_POINT ( 'NONE', #5243 ) ;
#18438 = CARTESIAN_POINT ( 'NONE',  ( 25.00000000000000000, 2.499999999999998668, -17.00000000000000000 ) ) ;
#18439 = B_SPLINE_CURVE_WITH_KNOTS ( 'NONE', 3,
 ( #10407, #16242, #7655, #14899, #14991, #15090 ),
 .UNSPECIFIED., .F., .F.,
 ( 4, 2, 4 ),
 ( 8.673617379884035472E-19, 0.001500839035891548753, 0.003001678071783096639 ),
 .UNSPECIFIED. ) ;
#18440 = EDGE_CURVE ( 'NONE', #204, #12842, #14810, .T. ) ;
#18441 = DIRECTION ( 'NONE',  ( -0.7635533937278216055, -0.5347026451755912957, -0.3620487483322542555 ) ) ;
#18442 = DIRECTION ( 'NONE',  ( 0.000000000000000000, 0.000000000000000000, 1.000000000000000000 ) ) ;
#18443 = CARTESIAN_POINT ( 'NONE',  ( 2.123976203522053741, 15.26039569100260174, 3.347755036805956763 ) ) ;
#18444 =( BOUNDED_SURFACE ( )  B_SPLINE_SURFACE ( 3, 1, ( 
 ( #16637, #10623 ),
 ( #9179, #769 ),
 ( #3439, #9550 ),
 ( #3539, #4787 ) ),
 .UNSPECIFIED., .F., .F., .T. ) 
 B_SPLINE_SURFACE_WITH_KNOTS ( ( 4, 4 ),
 ( 2, 2 ),
 ( 0.000000000000000000, 1.000000000000000000 ),
 ( 0.000000000000000000, 1.000000000000000000 ),
 .UNSPECIFIED. ) 
 GEOMETRIC_REPRESENTATION_ITEM ( )  RATIONAL_B_SPLINE_SURFACE ( (
 ( 1.000000000000000000, 1.000000000000000000),
 ( 0.9593108457356467333, 0.9995965569486454649),
 ( 0.9593108457356467333, 0.9995965569486454649),
 ( 1.000000000000000000, 1.000000000000000000) ) ) 
 REPRESENTATION_ITEM ( '' )  SURFACE ( )  );
#18445 = CARTESIAN_POINT ( 'NONE',  ( 2.636624412714756005, -2.161493821597335607, 15.91454522070219113 ) ) ;
#18446 =( NAMED_UNIT ( * ) PLANE_ANGLE_UNIT ( ) SI_UNIT ( $, .RADIAN. ) );
#18447 = CARTESIAN_POINT ( 'NONE',  ( 3.074695600507260984, -14.01296402267893448, 6.754521329824735076 ) ) ;
#18448 = CIRCLE ( 'NONE', #11142, 14.54644660717763927 ) ;
#18449 = CARTESIAN_POINT ( 'NONE',  ( 1.846138399168762101, 11.69739621335927815, -4.238866729160283064 ) ) ;
#18451 = ORIENTED_EDGE ( 'NONE', *, *, #16814, .T. ) ;
#18450 = CARTESIAN_POINT ( 'NONE',  ( 2.123976203522053297, 3.347755036805901252, 15.26039569100260884 ) ) ;
#18452 = CARTESIAN_POINT ( 'NONE',  ( 0.3170788640506440603, -11.02668139258435787, -8.200855617524654306 ) ) ;
#18453 = CARTESIAN_POINT ( 'NONE',  ( 0.4862570985993235340, 11.67702470553376060, -7.559321496869298329 ) ) ;
#18454 = CARTESIAN_POINT ( 'NONE',  ( 1.560000000000000053, -0.8660254037844384856, 1.500000000000000000 ) ) ;
#18455 = ORIENTED_EDGE ( 'NONE', *, *, #11319, .F. ) ;
#18456 = DIRECTION ( 'NONE',  ( 1.000000000000000000, 0.000000000000000000, 0.000000000000000000 ) ) ;
#18457 = CIRCLE ( 'NONE', #12660, 0.5000000000000004441 ) ;
#18458 = FACE_OUTER_BOUND ( 'NONE', #11002, .T. ) ;
#18459 = AXIS2_PLACEMENT_3D ( 'NONE', #16351, #6122, #3232 ) ;
#18460 = ORIENTED_EDGE ( 'NONE', *, *, #18778, .F. ) ;
#18461 = CYLINDRICAL_SURFACE ( 'NONE', #10491, 2.749999999999997335 ) ;
#18462 = VECTOR ( 'NONE', #7631, 999.9999999999998863 ) ;
#18463 = EDGE_CURVE ( 'NONE', #9556, #12864, #3907, .T. ) ;
#18464 = ADVANCED_FACE ( 'NONE', ( #3627 ), #14036, .F. ) ;
#18465 = ADVANCED_FACE ( 'NONE', ( #4970 ), #11774, .T. ) ;
#18466 = SURFACE_SIDE_STYLE ('',( #12820 ) ) ;
#18467 =( LENGTH_UNIT ( ) NAMED_UNIT ( * ) SI_UNIT ( .MILLI., .METRE. ) );
#18468 = CARTESIAN_POINT ( 'NONE',  ( 0.3145734862173242274, -11.29227530924451273, 7.825584895511488170 ) ) ;
#18469 = CARTESIAN_POINT ( 'NONE',  ( -108.0624185875376639, -81.60345299795268659, -90.16577778219220818 ) ) ;
#18470 = PRODUCT_CONTEXT ( 'NONE', #14862, 'mechanical' ) ;
#18471 =( LENGTH_UNIT ( ) NAMED_UNIT ( * ) SI_UNIT ( .MILLI., .METRE. ) );
#18472 = CARTESIAN_POINT ( 'NONE',  ( 3.950837973638668288, 0.000000000000000000, 0.000000000000000000 ) ) ;
#18473 = LINE ( 'NONE', #5554, #4209 ) ;
#18474 = VECTOR ( 'NONE', #2517, 1000.000000000000114 ) ;
#18475 = AXIS2_PLACEMENT_3D ( 'NONE', #3808, #8037, #15286 ) ;
#18476 = EDGE_CURVE ( 'NONE', #2296, #8583, #13896, .T. ) ;
#18477 = CARTESIAN_POINT ( 'NONE',  ( 1.846613052777651198, -4.166957398589769213, -11.72395935470502870 ) ) ;
#18478 = DIRECTION ( 'NONE',  ( -1.000000000000000000, -0.000000000000000000, -0.000000000000000000 ) ) ;
#18479 = CARTESIAN_POINT ( 'NONE',  ( 0.000000000000000000, 0.000000000000000000, 0.000000000000000000 ) ) ;
#18480 = DIRECTION ( 'NONE',  ( -1.000000000000000000, -1.239088197126290570E-16, 0.000000000000000000 ) ) ;
#18481 = SURFACE_STYLE_USAGE ( .BOTH. , #12929 ) ;
#18482 = ORIENTED_EDGE ( 'NONE', *, *, #16255, .F. ) ;
#18483 = EDGE_LOOP ( 'NONE', ( #12152, #13392, #6534, #14388 ) ) ;
#18484 = B_SPLINE_CURVE_WITH_KNOTS ( 'NONE', 3,
 ( #5400, #13815, #2343, #12296, #8278, #7920 ),
 .UNSPECIFIED., .F., .F.,
 ( 4, 2, 4 ),
 ( 1.748223473168675632E-18, 0.0002017457492448079337, 0.0004034914984896141327 ),
 .UNSPECIFIED. ) ;
#18485 = ORIENTED_EDGE ( 'NONE', *, *, #14670, .F. ) ;
#18486 = ORIENTED_EDGE ( 'NONE', *, *, #18401, .T. ) ;
#18487 = CARTESIAN_POINT ( 'NONE',  ( 0.000000000000000000, 0.000000000000000000, -12.00000000000000000 ) ) ;
#18488 = DIRECTION ( 'NONE',  ( 0.000000000000000000, 0.000000000000000000, 1.000000000000000000 ) ) ;
#18489 = AXIS2_PLACEMENT_3D ( 'NONE', #3048, #16556, #1735 ) ;
#18490 = ADVANCED_FACE ( 'NONE', ( #2111 ), #17002, .T. ) ;
#18491 = CARTESIAN_POINT ( 'NONE',  ( 3.664313757352971823, 7.012524439851495650, 12.42002390572628201 ) ) ;
#18492 = CARTESIAN_POINT ( 'NONE',  ( 2.002547531651519996, 6.845637710436190737, 10.57595306287294612 ) ) ;
#18493 = CARTESIAN_POINT ( 'NONE',  ( -26.50000000000001066, -12.50000000000000178, 7.000000000000000000 ) ) ;
#18494 = DIRECTION ( 'NONE',  ( -0.000000000000000000, -0.000000000000000000, -1.000000000000000000 ) ) ;
#18495 = CARTESIAN_POINT ( 'NONE',  ( 16.58200780006414732, 0.01115192838421568376, 0.0006320991582350033409 ) ) ;
#18496 = CARTESIAN_POINT ( 'NONE',  ( 2.636624412714236865, 0.000000000000000000, 0.000000000000000000 ) ) ;
#18497 = EDGE_CURVE ( 'NONE', #14481, #4102, #17884, .T. ) ;
#18498 = EDGE_LOOP ( 'NONE', ( #10531, #2395 ) ) ;
#18499 = VECTOR ( 'NONE', #9215, 1000.000000000000114 ) ;
#18500 = B_SPLINE_CURVE_WITH_KNOTS ( 'NONE', 3,
 ( #8055, #7876, #13863, #12255, #15301, #13688 ),
 .UNSPECIFIED., .F., .F.,
 ( 4, 2, 4 ),
 ( 0.000000000000000000, 0.001657017934710632240, 0.003314035869421264480 ),
 .UNSPECIFIED. ) ;
#18501 = ORIENTED_EDGE ( 'NONE', *, *, #4521, .T. ) ;
#18502 = EDGE_LOOP ( 'NONE', ( #641, #18578, #14092 ) ) ;
#18503 = ORIENTED_EDGE ( 'NONE', *, *, #2782, .T. ) ;
#18504 = DIRECTION ( 'NONE',  ( 0.000000000000000000, 0.000000000000000000, 1.000000000000000000 ) ) ;
#18505 = CIRCLE ( 'NONE', #16697, 8.767949192431130356 ) ;
#18506 = DIRECTION ( 'NONE',  ( 0.000000000000000000, -0.5000000000000003331, -0.8660254037844383745 ) ) ;
#18507 = CARTESIAN_POINT ( 'NONE',  ( 3.950837973638675393, 6.888253895133292559, 12.81214529934977797 ) ) ;
#18508 = CARTESIAN_POINT ( 'NONE',  ( 16.56822296793089322, -0.0007467251401297892322, -0.01011126603341077311 ) ) ;
#18509 = CARTESIAN_POINT ( 'NONE',  ( 16.57778382496167424, 0.01306626476309289374, -0.007244066302946823403 ) ) ;
#18510 = ORIENTED_EDGE ( 'NONE', *, *, #3804, .T. ) ;
#18511 = CARTESIAN_POINT ( 'NONE',  ( 1.847247051441594179, 9.967131402978196775, 7.448813758297206711 ) ) ;
#18512 = CIRCLE ( 'NONE', #214, 2.500000000000000000 ) ;
#18513 = VECTOR ( 'NONE', #10625, 1000.000000000000000 ) ;
#18514 = CARTESIAN_POINT ( 'NONE',  ( 0.3137051932979792457, -11.37800749014136592, 7.698472063774431717 ) ) ;
#18515 = CARTESIAN_POINT ( 'NONE',  ( 4.238775304281403145, 7.500000000000264677, -13.18441022661325945 ) ) ;
#18516 = CARTESIAN_POINT ( 'NONE',  ( 1.560000000000000053, 1.732050807568878747, 7.017607234860990640E-28 ) ) ;
#18517 = VECTOR ( 'NONE', #17221, 1000.000000000000114 ) ;
#18518 = DIRECTION ( 'NONE',  ( -1.000000000000000000, -0.000000000000000000, -0.000000000000000000 ) ) ;
#18519 = AXIS2_PLACEMENT_3D ( 'NONE', #3149, #15016, #4801 ) ;
#18520 = DIRECTION ( 'NONE',  ( 0.000000000000000000, 0.000000000000000000, 1.000000000000000000 ) ) ;
#18521 = DIRECTION ( 'NONE',  ( -1.000000000000000000, 0.000000000000000000, 0.000000000000000000 ) ) ;
#18522 = B_SPLINE_CURVE_WITH_KNOTS ( 'NONE', 3,
 ( #18297, #14957, #814, #634, #12100, #5114 ),
 .UNSPECIFIED., .F., .F.,
 ( 4, 2, 4 ),
 ( 3.490137563248181679E-18, 0.0002017457492448096685, 0.0004034914984896158133 ),
 .UNSPECIFIED. ) ;
#18523 = EDGE_CURVE ( 'NONE', #17807, #16214, #5636, .T. ) ;
#18524 = DIRECTION ( 'NONE',  ( -0.7561779333270775005, -0.6534392409364822019, 0.03481510524964565034 ) ) ;
#18525 = ORIENTED_EDGE ( 'NONE', *, *, #11571, .F. ) ;
#18526 = CONICAL_SURFACE ( 'NONE', #16714, 14.54644660717763927, 0.8559913436420816257 ) ;
#18528 = ORIENTED_EDGE ( 'NONE', *, *, #14729, .F. ) ;
#18527 = DIRECTION ( 'NONE',  ( 1.000000000000000000, 0.000000000000000000, 0.000000000000000000 ) ) ;
#18529 = FACE_OUTER_BOUND ( 'NONE', #12535, .T. ) ;
#18530 = AXIS2_PLACEMENT_3D ( 'NONE', #17720, #14737, #8909 ) ;
#18531 = ADVANCED_FACE ( 'NONE', ( #761 ), #3532, .T. ) ;
#18532 = CARTESIAN_POINT ( 'NONE',  ( 16.56753206892534891, 0.006669401563385194548, 0.006760771273035138390 ) ) ;
#18533 = ORIENTED_EDGE ( 'NONE', *, *, #14431, .T. ) ;
#18534 = CARTESIAN_POINT ( 'NONE',  ( 0.4862570985993235340, -13.44146924561383827, 3.580942890621619412 ) ) ;
#18535 = CARTESIAN_POINT ( 'NONE',  ( -6.538348415310989203, -7.500000000000000000, -12.00000000000006040 ) ) ;
#18536 = CARTESIAN_POINT ( 'NONE',  ( 0.3095370825347233956, 13.20347358821914519, 3.806662003783457315 ) ) ;
#18537 = VERTEX_POINT ( 'NONE', #16813 ) ;
#18538 = DIRECTION ( 'NONE',  ( -0.000000000000000000, -0.5000000000000003331, -0.8660254037844384856 ) ) ;
#18539 = AXIS2_PLACEMENT_3D ( 'NONE', #7832, #565, #12393 ) ;
#18540 = CARTESIAN_POINT ( 'NONE',  ( 0.4862570985993235340, -11.67702470553359539, -7.559321496869553236 ) ) ;
#18541 = CARTESIAN_POINT ( 'NONE',  ( 1.846524061778019199, 12.43723828841088341, 0.3544704288992919228 ) ) ;
#18542 = DIRECTION ( 'NONE',  ( -1.000000000000000000, -0.000000000000000000, -0.000000000000000000 ) ) ;
#18543 = CARTESIAN_POINT ( 'NONE',  ( 1.847461586945732703, 11.84459954310610463, 3.813310247068479431 ) ) ;
#18544 =( NAMED_UNIT ( * ) SI_UNIT ( $, .STERADIAN. ) SOLID_ANGLE_UNIT ( ) );
#18545 = EDGE_CURVE ( 'NONE', #16692, #7133, #1077, .T. ) ;
#18546 = DIRECTION ( 'NONE',  ( 0.000000000000000000, 1.000000000000000000, -0.000000000000000000 ) ) ;
#18547 = CARTESIAN_POINT ( 'NONE',  ( 0.4862570985993235340, -0.7479633556563419772, 13.89016912371017121 ) ) ;
#18549 = VERTEX_POINT ( 'NONE', #9545 ) ;
#18548 = CARTESIAN_POINT ( 'NONE',  ( 16.58200780006414732, -0.007066318000005944282, 0.008650561019685880718 ) ) ;
#18550 = CARTESIAN_POINT ( 'NONE',  ( 0.3939822652208109788, 0.7002900021919884477, -13.80035637018651684 ) ) ;
#18551 = VECTOR ( 'NONE', #13043, 1000.000000000000000 ) ;
#18552 = EDGE_CURVE ( 'NONE', #12155, #16968, #3752, .T. ) ;
#18553 = PLANE ( 'NONE',  #6480 ) ;
#18554 = ORIENTED_EDGE ( 'NONE', *, *, #12749, .F. ) ;
#18555 = DIRECTION ( 'NONE',  ( -1.000000000000000000, 0.000000000000000000, 0.000000000000000000 ) ) ;
#18556 = CARTESIAN_POINT ( 'NONE',  ( 1.846138399168762101, 10.30487220521580305, -6.971848976710897539 ) ) ;
#18557 = EDGE_LOOP ( 'NONE', ( #3219, #8185, #13144, #14181 ) ) ;
#18558 = CARTESIAN_POINT ( 'NONE',  ( 0.3132642857406540138, -4.743831191224475496, 12.89240536501344536 ) ) ;
#18559 = CARTESIAN_POINT ( 'NONE',  ( 16.56872352241294521, 0.007512283835805451566, 0.007240717549634016065 ) ) ;
#18560 = LINE ( 'NONE', #2682, #10672 ) ;
#18561 = CARTESIAN_POINT ( 'NONE',  ( 1.845755665166724180, 7.694641135842960722, -9.776700214453546423 ) ) ;
#18562 = LINE ( 'NONE', #12736, #18517 ) ;
#18563 = ORIENTED_EDGE ( 'NONE', *, *, #15715, .F. ) ;
#18564 = CONTEXT_DEPENDENT_SHAPE_REPRESENTATION ( #5944, #16708 ) ;
#18565 =( NAMED_UNIT ( * ) SI_UNIT ( $, .STERADIAN. ) SOLID_ANGLE_UNIT ( ) );
#18566 = CARTESIAN_POINT ( 'NONE',  ( 1.918921323896324749, 7.860085869556325378, -9.738309537478915701 ) ) ;
#18568 = EDGE_LOOP ( 'NONE', ( #7406, #1602, #15011, #8630 ) ) ;
#18567 = CARTESIAN_POINT ( 'NONE',  ( 1.845755665166725068, -0.4784952423729416648, 12.43231320373360838 ) ) ;
#18569 = CARTESIAN_POINT ( 'NONE',  ( 1.847034903785823134, -3.625649561595226888, -11.90269060117937627 ) ) ;
#18570 = CARTESIAN_POINT ( 'NONE',  ( 1.847461586945732925, 3.877048136045379234, 11.82388984758120287 ) ) ;
#18571 = DIRECTION ( 'NONE',  ( 0.000000000000000000, 1.000000000000000000, 0.000000000000000000 ) ) ;
#18572 = ADVANCED_FACE ( 'NONE', ( #12869 ), #10005, .F. ) ;
#18573 = ORIENTED_EDGE ( 'NONE', *, *, #10115, .T. ) ;
#18574 = CARTESIAN_POINT ( 'NONE',  ( 0.3095370825347233956, -3.806662003783505277, 13.20347358821913275 ) ) ;
#18575 = ORIENTED_EDGE ( 'NONE', *, *, #2706, .F. ) ;
#18576 = EDGE_LOOP ( 'NONE', ( #2219, #1839, #8734, #1541 ) ) ;
#18577 = ORIENTED_EDGE ( 'NONE', *, *, #10379, .F. ) ;
#18578 = ORIENTED_EDGE ( 'NONE', *, *, #15909, .F. ) ;
#18579 = CARTESIAN_POINT ( 'NONE',  ( 2.636624412714237309, 11.10302021257826866, 11.60464335004050973 ) ) ;
#18580 = CARTESIAN_POINT ( 'NONE',  ( 1.560000000000000053, 0.000000000000000000, 1.500000000000000000 ) ) ;
#18581 = CARTESIAN_POINT ( 'NONE',  ( 1.560000000000000053, 0.8660254037844389297, 1.500000000000000000 ) ) ;
#18582 = CARTESIAN_POINT ( 'NONE',  ( 0.3137051932979792457, -10.83767969834796929, -8.442169467526971616 ) ) ;
#18583 = CARTESIAN_POINT ( 'NONE',  ( 1.560000000000000053, 0.000000000000000000, 0.000000000000000000 ) ) ;
#18584 = CARTESIAN_POINT ( 'NONE',  ( 16.57778382496167424, -0.01354073047775762942, -0.006312874906843820091 ) ) ;
#18585 = CIRCLE ( 'NONE', #5174, 16.06066017081991149 ) ;
#18586 = CARTESIAN_POINT ( 'NONE',  ( 1.342453679581834924, -9.456403821038714241, -11.38190519890864039 ) ) ;
#18587 = EDGE_CURVE ( 'NONE', #9121, #11277, #18772, .T. ) ;
#18588 = CARTESIAN_POINT ( 'NONE',  ( 1.918918678667072442, -12.49849921341423276, 0.6348738215464800883 ) ) ;
#18589 = EDGE_CURVE ( 'NONE', #4298, #15356, #2641, .T. ) ;
#18590 = ORIENTED_EDGE ( 'NONE', *, *, #1312, .F. ) ;
#18591 = ADVANCED_FACE ( 'NONE', ( #12964 ), #5791, .T. ) ;
#18592 = ORIENTED_EDGE ( 'NONE', *, *, #14338, .T. ) ;
#18593 = VERTEX_POINT ( 'NONE', #9729 ) ;
#18594 = B_SPLINE_CURVE_WITH_KNOTS ( 'NONE', 3,
 ( #584, #9366, #10515, #8978, #13376, #6209 ),
 .UNSPECIFIED., .F., .F.,
 ( 4, 2, 4 ),
 ( 8.673617379884035472E-19, 0.0001828790815886939666, 0.0003657581631773870658 ),
 .UNSPECIFIED. ) ;
#18595 = ORIENTED_EDGE ( 'NONE', *, *, #11066, .F. ) ;
#18596 = DIRECTION ( 'NONE',  ( -0.000000000000000000, 0.000000000000000000, 1.000000000000000000 ) ) ;
#18597 = FACE_OUTER_BOUND ( 'NONE', #18425, .T. ) ;
#18598 = CARTESIAN_POINT ( 'NONE',  ( 2.002547531651519996, -11.75462648437105173, 4.532360870844282630 ) ) ;
#18599 = CARTESIAN_POINT ( 'NONE',  ( 0.000000000000000000, 0.8660254037844389297, 1.500000000000000000 ) ) ;
#18600 = CARTESIAN_POINT ( 'NONE',  ( 1.847380140988742925, -7.224522571381399416, 10.13114603776194045 ) ) ;
#18601 = ORIENTED_EDGE ( 'NONE', *, *, #2524, .T. ) ;
#18602 = CARTESIAN_POINT ( 'NONE',  ( 2.636624412714236865, 0.000000000000000000, 0.000000000000000000 ) ) ;
#18603 = CARTESIAN_POINT ( 'NONE',  ( 1.846138399168762101, -4.238866729160323032, -11.69739621335926394 ) ) ;
#18604 = CARTESIAN_POINT ( 'NONE',  ( 5.275788075193746707, 7.499999999999999112, -12.98022329939734298 ) ) ;
#18605 = LINE ( 'NONE', #11448, #3334 ) ;
#18606 = CARTESIAN_POINT ( 'NONE',  ( 0.000000000000000000, 9.999999999999973355, -2.000000000000000000 ) ) ;
#18607 = DIRECTION ( 'NONE',  ( -1.000000000000000000, 0.000000000000000000, -0.000000000000000000 ) ) ;
#18608 = CARTESIAN_POINT ( 'NONE',  ( 0.4862570985993252548, 5.003653737315486794, 12.97920246947881395 ) ) ;
#18609 = LINE ( 'NONE', #17370, #15209 ) ;
#18610 = VERTEX_POINT ( 'NONE', #2453 ) ;
#18612 = VERTEX_POINT ( 'NONE', #11273 ) ;
#18611 = CARTESIAN_POINT ( 'NONE',  ( -199.9999999999999716, -5.000000000000024869, 6.000000000000005329 ) ) ;
#18613 = FACE_OUTER_BOUND ( 'NONE', #3593, .T. ) ;
#18614 = EDGE_CURVE ( 'NONE', #492, #10356, #9900, .T. ) ;
#18615 = ORIENTED_EDGE ( 'NONE', *, *, #10655, .T. ) ;
#18616 = ADVANCED_FACE ( 'NONE', ( #11638 ), #11567, .F. ) ;
#18617 = DIRECTION ( 'NONE',  ( -1.000000000000000000, -0.000000000000000000, -0.000000000000000000 ) ) ;
#18618 = VERTEX_POINT ( 'NONE', #17366 ) ;
#18619 = DIRECTION ( 'NONE',  ( 0.7561779333270775005, 0.5491072561318364187, -0.3559159372837296664 ) ) ;
#18620 = CARTESIAN_POINT ( 'NONE',  ( -199.9999999999999716, 4.999999999999973355, 3.000000000000000000 ) ) ;
#18621 = FACE_OUTER_BOUND ( 'NONE', #6638, .T. ) ;
#18622 = PRESENTATION_STYLE_ASSIGNMENT (( #12799 ) ) ;
#18623 = EDGE_LOOP ( 'NONE', ( #16731, #2458 ) ) ;
#18624 = CARTESIAN_POINT ( 'NONE',  ( 1.846138399168762989, -3.446241763653083101, 11.95493567637849530 ) ) ;
#18625 = DIRECTION ( 'NONE',  ( -1.000000000000000000, 0.000000000000000000, 0.000000000000000000 ) ) ;
#18626 = CARTESIAN_POINT ( 'NONE',  ( -194.9999999999999716, -5.000000000000024869, 3.000000000000000000 ) ) ;
#18627 = CARTESIAN_POINT ( 'NONE',  ( 12.00000000000000711, -19.99999999999999645, 8.000000000000000000 ) ) ;
#18628 = CARTESIAN_POINT ( 'NONE',  ( 1.560000000000000053, 0.000000000000000000, 0.000000000000000000 ) ) ;
#18629 = EDGE_CURVE ( 'NONE', #7718, #8099, #18773, .T. ) ;
#18630 =( LENGTH_UNIT ( ) NAMED_UNIT ( * ) SI_UNIT ( .MILLI., .METRE. ) );
#18631 = CARTESIAN_POINT ( 'NONE',  ( 15.00000000000000711, -19.99999999999999645, 8.000000000000000000 ) ) ;
#18632 = CIRCLE ( 'NONE', #4933, 4.750000000000000000 ) ;
#18633 = PRODUCT_RELATED_PRODUCT_CATEGORY ( 'part', '', ( #15013 ) ) ;
#18634 = ADVANCED_FACE ( 'NONE', ( #12689 ), #14210, .T. ) ;
#18635 = DIRECTION ( 'NONE',  ( -0.000000000000000000, -0.5000000000000004441, 0.8660254037844383745 ) ) ;
#18637 = ORIENTED_EDGE ( 'NONE', *, *, #16564, .T. ) ;
#18636 = CARTESIAN_POINT ( 'NONE',  ( 2.747332970342022840, 2.705255688517843371, 16.12459247543627683 ) ) ;
#18638 = PLANE ( 'NONE',  #9391 ) ;
#18639 = B_SPLINE_CURVE_WITH_KNOTS ( 'NONE', 3,
 ( #16149, #5714, #5812, #4109, #15760, #11753 ),
 .UNSPECIFIED., .F., .F.,
 ( 4, 2, 4 ),
 ( 4.336808689942017736E-19, 0.0001828790815886937498, 0.0003657581631773870658 ),
 .UNSPECIFIED. ) ;
#18640 = EDGE_CURVE ( 'NONE', #11305, #11392, #7878, .T. ) ;
#18641 = CARTESIAN_POINT ( 'NONE',  ( 3.377929128793396352, -12.02809354424095822, -7.136734442940969814 ) ) ;
#18642 = ORIENTED_EDGE ( 'NONE', *, *, #12615, .T. ) ;
#18643 = CARTESIAN_POINT ( 'NONE',  ( 7.000000000000000000, 8.572527594031473190E-16, 8.000000000000000000 ) ) ;
#18644 = CARTESIAN_POINT ( 'NONE',  ( 0.3148213771069364175, 0.2297580318216631001, -13.73693585713733967 ) ) ;
#18645 = VERTEX_POINT ( 'NONE', #12781 ) ;
#18646 = FACE_OUTER_BOUND ( 'NONE', #3168, .T. ) ;
#18647 = CARTESIAN_POINT ( 'NONE',  ( 0.3308579732647051186, 3.680601586799872482, 13.25341063505876882 ) ) ;
#18648 = DIRECTION ( 'NONE',  ( 1.000000000000000000, 1.298018465182616140E-16, -0.000000000000000000 ) ) ;
#18649 = DIRECTION ( 'NONE',  ( 0.000000000000000000, 0.000000000000000000, 1.000000000000000000 ) ) ;
#18650 = EDGE_CURVE ( 'NONE', #17449, #2783, #9916, .T. ) ;
#18651 = EDGE_LOOP ( 'NONE', ( #9903, #7312, #13658, #4121 ) ) ;
#18652 =( NAMED_UNIT ( * ) PLANE_ANGLE_UNIT ( ) SI_UNIT ( $, .RADIAN. ) );
#18653 = CYLINDRICAL_SURFACE ( 'NONE', #5285, 10.00000000000000888 ) ;
#18654 = EDGE_CURVE ( 'NONE', #12518, #12767, #11455, .T. ) ;
#18655 = CARTESIAN_POINT ( 'NONE',  ( 3.512766787570772653, -2.682019731918489303, 14.81029789862156143 ) ) ;
#18656 = CARTESIAN_POINT ( 'NONE',  ( 0.3939875929385652231, -10.75308190953749410, 8.678227324501083473 ) ) ;
#18657 = CARTESIAN_POINT ( 'NONE',  ( 1.846138399168762989, 3.446241763652997836, 11.95493567637851839 ) ) ;
#18658 = DIRECTION ( 'NONE',  ( -1.000000000000000000, -0.000000000000000000, -0.000000000000000000 ) ) ;
#18659 = EDGE_LOOP ( 'NONE', ( #16529, #6179 ) ) ;
#18660 = CARTESIAN_POINT ( 'NONE',  ( 0.3151930723728382788, 11.16020735774779027, -8.013866567350774517 ) ) ;
#18661 = CARTESIAN_POINT ( 'NONE',  ( 1.918918678667046684, -7.860057224348774518, -9.738328798462466906 ) ) ;
#18662 = ORIENTED_EDGE ( 'NONE', *, *, #17019, .F. ) ;
#18663 = ORIENTED_EDGE ( 'NONE', *, *, #1715, .F. ) ;
#18664 = LINE ( 'NONE', #1563, #11398 ) ;
#18665 = ORIENTED_EDGE ( 'NONE', *, *, #18629, .F. ) ;
#18666 = CARTESIAN_POINT ( 'NONE',  ( 0.3151928479966097374, 1.775918418904422640E-15, 13.73922861026898623 ) ) ;
#18667 = AXIS2_PLACEMENT_3D ( 'NONE', #14628, #13190, #9183 ) ;
#18668 = ORIENTED_EDGE ( 'NONE', *, *, #18094, .F. ) ;
#18669 = CARTESIAN_POINT ( 'NONE',  ( 1.846138399168762989, 3.446241763652997836, 11.95493567637851839 ) ) ;
#18670 = CARTESIAN_POINT ( 'NONE',  ( 0.3151926232592466293, 13.04305446098362253, -4.318679262939488339 ) ) ;
#18671 = EDGE_CURVE ( 'NONE', #9678, #5818, #5598, .T. ) ;
#18672 = DIRECTION ( 'NONE',  ( -0.7635533937278216055, -0.6204116510013465424, -0.1790966170213987851 ) ) ;
#18673 = DIRECTION ( 'NONE',  ( -1.000000000000000000, 0.000000000000000000, 0.000000000000000000 ) ) ;
#18674 = CARTESIAN_POINT ( 'NONE',  ( 16.56872352241294521, 0.01027347319884441834, -0.001821578298044677175 ) ) ;
#18675 = CARTESIAN_POINT ( 'NONE',  ( 2.636624412717099908, 11.60464335004051861, -11.10302021258208249 ) ) ;
#18676 = B_SPLINE_CURVE_WITH_KNOTS ( 'NONE', 3,
 ( #13396, #15019, #3256, #6142, #9101, #11874 ),
 .UNSPECIFIED., .F., .F.,
 ( 4, 2, 4 ),
 ( 0.000000000000000000, 0.001656992708823057468, 0.003313985417646114935 ),
 .UNSPECIFIED. ) ;
#18677 = VECTOR ( 'NONE', #3471, 1000.000000000000000 ) ;
#18678 = CARTESIAN_POINT ( 'NONE',  ( 2.002547531651519996, 6.845637710436190737, 10.57595306287294612 ) ) ;
#18679 = DIRECTION ( 'NONE',  ( 1.000000000000000000, -0.000000000000000000, -0.000000000000000000 ) ) ;
#18680 = VERTEX_POINT ( 'NONE', #13449 ) ;
#18681 = EDGE_LOOP ( 'NONE', ( #4534, #18486, #14263, #14184 ) ) ;
#18682 = ORIENTED_EDGE ( 'NONE', *, *, #18497, .F. ) ;
#18683 = ORIENTED_EDGE ( 'NONE', *, *, #9051, .F. ) ;
#18684 = VERTEX_POINT ( 'NONE', #13542 ) ;
#18685 = FACE_OUTER_BOUND ( 'NONE', #10088, .T. ) ;
#18686 = DIRECTION ( 'NONE',  ( 0.000000000000000000, 0.5000000000000003331, 0.8660254037844383745 ) ) ;
#18687 = CARTESIAN_POINT ( 'NONE',  ( 3.950837973638676281, 1.958075594453990487, -14.41405733518058341 ) ) ;
#18688 = EDGE_LOOP ( 'NONE', ( #3372, #887, #13571, #11912 ) ) ;
#18689 = CARTESIAN_POINT ( 'NONE',  ( 2.002547531651519996, 12.57989064830759496, 0.6781519942172178350 ) ) ;
#18690 = EDGE_CURVE ( 'NONE', #3191, #11533, #1510, .T. ) ;
#18691 = EDGE_CURVE ( 'NONE', #9212, #7718, #18342, .T. ) ;
#18692 = DIRECTION ( 'NONE',  ( 0.000000000000000000, 0.000000000000000000, 1.000000000000000000 ) ) ;
#18693 = EDGE_CURVE ( 'NONE', #11053, #13313, #8103, .T. ) ;
#18694 = CARTESIAN_POINT ( 'NONE',  ( 5.031681560115344176, 4.880796135282181147, -12.00000000472804196 ) ) ;
#18695 = CARTESIAN_POINT ( 'NONE',  ( 1.918921323896323639, -10.48468902844557071, 6.832782632379341692 ) ) ;
#18696 = AXIS2_PLACEMENT_3D ( 'NONE', #13018, #2869, #3059 ) ;
#18697 = DIRECTION ( 'NONE',  ( 0.000000000000000000, 0.000000000000000000, 1.000000000000000000 ) ) ;
#18698 = CARTESIAN_POINT ( 'NONE',  ( 1.845755665166725290, -10.33920510797148395, 6.920419570228313333 ) ) ;
#18699 = CARTESIAN_POINT ( 'NONE',  ( 16.56753206892534891, 0.008490833999798002782, -0.004253784598196794220 ) ) ;
#18700 = DIRECTION ( 'NONE',  ( -1.000000000000000000, -0.000000000000000000, -0.000000000000000000 ) ) ;
#18701 = ORIENTED_EDGE ( 'NONE', *, *, #6047, .F. ) ;
#18702 = ORIENTED_EDGE ( 'NONE', *, *, #12213, .T. ) ;
#18703 = CARTESIAN_POINT ( 'NONE',  ( 0.4754618798421171855, 10.80499583390525764, -8.775436892860993154 ) ) ;
#18704 = CARTESIAN_POINT ( 'NONE',  ( 0.3095370825347234511, 3.806662003783410242, 13.20347358821915940 ) ) ;
#18705 = VERTEX_POINT ( 'NONE', #270 ) ;
#18706 = CARTESIAN_POINT ( 'NONE',  ( 16.57210152137263393, 0.01214401161737623663, 0.008007331252333469568 ) ) ;
#18707 = CIRCLE ( 'NONE', #14749, 5.000000000000000000 ) ;
#18708 = AXIS2_PLACEMENT_3D ( 'NONE', #15728, #8477, #1205 ) ;
#18709 = ORIENTED_EDGE ( 'NONE', *, *, #2079, .T. ) ;
#18710 = DIRECTION ( 'NONE',  ( 0.000000000000000000, 0.000000000000000000, 1.000000000000000000 ) ) ;
#18711 = DIRECTION ( 'NONE',  ( -1.000000000000000000, -0.000000000000000000, -0.000000000000000000 ) ) ;
#18712 = FACE_OUTER_BOUND ( 'NONE', #4536, .T. ) ;
#18714 = CARTESIAN_POINT ( 'NONE',  ( 16.58200780006414732, 0.01041078477704048856, 0.004047297414159084679 ) ) ;
#18713 =( BOUNDED_SURFACE ( )  B_SPLINE_SURFACE ( 3, 1, ( 
 ( #6349, #14935 ),
 ( #3463, #9297 ),
 ( #6532, #416 ),
 ( #10936, #13597 ) ),
 .UNSPECIFIED., .F., .F., .T. ) 
 B_SPLINE_SURFACE_WITH_KNOTS ( ( 4, 4 ),
 ( 2, 2 ),
 ( 0.000000000000000000, 1.000000000000000000 ),
 ( 0.000000000000000000, 1.000000000000000000 ),
 .UNSPECIFIED. ) 
 GEOMETRIC_REPRESENTATION_ITEM ( )  RATIONAL_B_SPLINE_SURFACE ( (
 ( 1.000000000000000000, 1.000000000000000000),
 ( 0.7792777138730160313, 0.9689936506012927220),
 ( 0.7792777138730160313, 0.9689936506012927220),
 ( 1.000000000000000000, 1.000000000000000000) ) ) 
 REPRESENTATION_ITEM ( '' )  SURFACE ( )  );
#18715 = ORIENTED_EDGE ( 'NONE', *, *, #7100, .T. ) ;
#18716 = CARTESIAN_POINT ( 'NONE',  ( 16.56679352167444819, -0.009190982326619729845, -0.001390132774594407148 ) ) ;
#18717 = DIRECTION ( 'NONE',  ( 0.000000000000000000, 0.000000000000000000, -1.000000000000000000 ) ) ;
#18718 = CARTESIAN_POINT ( 'NONE',  ( 0.000000000000000000, 3.061616997868383141E-16, -2.500000000000000000 ) ) ;
#18719 = CARTESIAN_POINT ( 'NONE',  ( 0.3150692679895995552, -13.01874238516607285, -4.391039771493804089 ) ) ;
#18720 = CARTESIAN_POINT ( 'NONE',  ( -4.999999999999995559, -30.00000000000000000, 26.00000000000000000 ) ) ;
#18721 = CARTESIAN_POINT ( 'NONE',  ( 1.846138399168762101, 6.971848976711011225, 10.30487220521572667 ) ) ;
#18722 = ADVANCED_FACE ( 'NONE', ( #10591 ), #7349, .T. ) ;
#18723 = DIRECTION ( 'NONE',  ( 0.000000000000000000, 0.000000000000000000, 1.000000000000000000 ) ) ;
#18724 = DIRECTION ( 'NONE',  ( -0.7635533937278216055, -0.5095610256143884298, 0.3966532189476580372 ) ) ;
#18725 = AXIS2_PLACEMENT_3D ( 'NONE', #12803, #18717, #18625 ) ;
#18726 = TOROIDAL_SURFACE ( 'NONE', #17837, 11.50000000000000178, 0.5000000000000000000 ) ;
#18727 = AXIS2_PLACEMENT_3D ( 'NONE', #8554, #3882, #6842 ) ;
#18728 = CARTESIAN_POINT ( 'NONE',  ( 1.847412631396503357, 7.348689888531986014, -10.04119192206678512 ) ) ;
#18730 = ORIENTED_EDGE ( 'NONE', *, *, #1532, .T. ) ;
#18729 = CARTESIAN_POINT ( 'NONE',  ( 2.636624412714236865, 0.000000000000000000, 0.000000000000000000 ) ) ;
#18731 = LINE ( 'NONE', #7187, #17624 ) ;
#18732 = ADVANCED_FACE ( 'NONE', ( #16026 ), #3199, .T. ) ;
#18733 = DIRECTION ( 'NONE',  ( -1.000000000000000000, -0.000000000000000000, -0.000000000000000000 ) ) ;
#18734 = B_SPLINE_CURVE_WITH_KNOTS ( 'NONE', 3,
 ( #2484, #8159, #3843, #12623, #8339, #8252, #1058, #2314, #18367, #13974, #16937, #883, #6724 ),
 .UNSPECIFIED., .F., .F.,
 ( 4, 3, 3, 3, 4 ),
 ( 3.878959614448864246E-18, 0.0002299780670421054142, 0.0004599561239687919093, 0.0006896788984287899067, 0.0009194956271626406052 ),
 .UNSPECIFIED. ) ;
#18735 = ORIENTED_EDGE ( 'NONE', *, *, #1264, .F. ) ;
#18736 = CARTESIAN_POINT ( 'NONE',  ( 16.56753206892534891, -0.001549402974394229436, -0.009369540855502527313 ) ) ;
#18737 = CARTESIAN_POINT ( 'NONE',  ( 0.4862570985993235340, -5.003653737315397976, -12.97920246947884770 ) ) ;
#18738 = ORIENTED_EDGE ( 'NONE', *, *, #14977, .T. ) ;
#18739 = CARTESIAN_POINT ( 'NONE',  ( 16.56679352167444819, -0.008252760440870528930, -0.004277682826582232013 ) ) ;
#18740 = CARTESIAN_POINT ( 'NONE',  ( 1.846822687350014869, -9.891732594446525084, -7.547953575784235092 ) ) ;
#18741 = ADVANCED_FACE ( 'NONE', ( #7641 ), #5890, .T. ) ;
#18742 = DIRECTION ( 'NONE',  ( 0.000000000000000000, 0.000000000000000000, 1.000000000000000000 ) ) ;
#18743 = CARTESIAN_POINT ( 'NONE',  ( 3.950837973638677170, 6.316429227969654114, -13.10350451991833687 ) ) ;
#18744 = ORIENTED_EDGE ( 'NONE', *, *, #10780, .F. ) ;
#18745 = ADVANCED_FACE ( 'NONE', ( #10393 ), #13294, .F. ) ;
#18746 = ADVANCED_FACE ( 'NONE', ( #3110 ), #7732, .T. ) ;
#18747 = DIRECTION ( 'NONE',  ( 0.000000000000000000, 0.000000000000000000, 1.000000000000000000 ) ) ;
#18748 = DIRECTION ( 'NONE',  ( 0.000000000000000000, 0.000000000000000000, 1.000000000000000000 ) ) ;
#18749 = EDGE_CURVE ( 'NONE', #9990, #8563, #8764, .T. ) ;
#18750 = CARTESIAN_POINT ( 'NONE',  ( 2.636624412714237309, 7.605649742761960042, 14.14563173255213613 ) ) ;
#18751 = CARTESIAN_POINT ( 'NONE',  ( 1.846613052777651198, 4.166957398589849149, 11.72395935470500028 ) ) ;
#18752 = CARTESIAN_POINT ( 'NONE',  ( 16.56753206892534891, 0.001549402974393146101, -0.009369540855502138735 ) ) ;
#18753 = VECTOR ( 'NONE', #8856, 1000.000000000000000 ) ;
#18754 = APPLICATION_CONTEXT ( 'automotive_design' ) ;
#18755 = ORIENTED_EDGE ( 'NONE', *, *, #8602, .F. ) ;
#18756 = CARTESIAN_POINT ( 'NONE',  ( 0.4862570985993235340, -13.44146924561378498, -3.580942890621813923 ) ) ;
#18757 = CARTESIAN_POINT ( 'NONE',  ( 16.56782317627811096, -0.0003415813796015412622, -0.009814734722106366327 ) ) ;
#18758 = AXIS2_PLACEMENT_3D ( 'NONE', #4114, #8511, #9935 ) ;
#18759 = B_SPLINE_CURVE_WITH_KNOTS ( 'NONE', 3,
 ( #2089, #7925, #5031, #857, #6504, #7956 ),
 .UNSPECIFIED., .F., .F.,
 ( 4, 2, 4 ),
 ( 0.000000000000000000, 0.001656992708823243950, 0.003313985417646487033 ),
 .UNSPECIFIED. ) ;
#18760 = ORIENTED_EDGE ( 'NONE', *, *, #12749, .T. ) ;
#18761 = VECTOR ( 'NONE', #18057, 1000.000000000000000 ) ;
#18762 = EDGE_CURVE ( 'NONE', #12765, #7766, #10300, .T. ) ;
#18763 = ORIENTED_EDGE ( 'NONE', *, *, #1420, .T. ) ;
#18764 = CARTESIAN_POINT ( 'NONE',  ( 0.3939875929385635578, -4.930599594904470528, -12.90850834464105645 ) ) ;
#18765 = ORIENTED_EDGE ( 'NONE', *, *, #10782, .F. ) ;
#18766 = CARTESIAN_POINT ( 'NONE',  ( 0.3151928479966097929, -0.07658992383253612757, 13.73922861026898623 ) ) ;
#18767 = ORIENTED_EDGE ( 'NONE', *, *, #16809, .F. ) ;
#18768 = CARTESIAN_POINT ( 'NONE',  ( 2.320521194581854907, 10.64885423995017355, 11.60169518685927059 ) ) ;
#18769 = CARTESIAN_POINT ( 'NONE',  ( 1.847247051441587518, -9.967131402978145260, -7.448813758297282206 ) ) ;
#18770 = CIRCLE ( 'NONE', #10859, 5.000000000000000888 ) ;
#18771 = CARTESIAN_POINT ( 'NONE',  ( -6.000000000000000888, 17.00000000000000000, 4.000000000000000000 ) ) ;
#18772 = CIRCLE ( 'NONE', #782, 5.000000000000000000 ) ;
#18773 = B_SPLINE_CURVE_WITH_KNOTS ( 'NONE', 3,
 ( #14119, #1025, #1408, #8666, #4282, #7252 ),
 .UNSPECIFIED., .F., .F.,
 ( 4, 2, 4 ),
 ( 8.673617379884035472E-19, 0.0001828790815886931534, 0.0003657581631773854395 ),
 .UNSPECIFIED. ) ;
#18774 = CARTESIAN_POINT ( 'NONE',  ( 3.950837973638676281, -6.316429227969383220, -13.10350451991847009 ) ) ;
#18775 = CARTESIAN_POINT ( 'NONE',  ( 0.4754618798421167414, -5.007009103465340338, 12.98792082933642966 ) ) ;
#18776 = CARTESIAN_POINT ( 'NONE',  ( 0.4754618798421167414, 8.775436892861268490, -10.80499583390503560 ) ) ;
#18777 = CARTESIAN_POINT ( 'NONE',  ( 16.56753206892534891, -0.009369540855502522109, 0.001549402974394263697 ) ) ;
#18778 = EDGE_CURVE ( 'NONE', #11575, #4533, #17427, .T. ) ;
#18779 = VERTEX_POINT ( 'NONE', #5220 ) ;
#18780 = VERTEX_POINT ( 'NONE', #16793 ) ;
#18781 = EDGE_CURVE ( 'NONE', #2339, #8095, #1940, .T. ) ;
#18782 = ORIENTED_EDGE ( 'NONE', *, *, #10596, .F. ) ;
#18783 = ORIENTED_EDGE ( 'NONE', *, *, #11937, .F. ) ;
#18784 = AXIS2_PLACEMENT_3D ( 'NONE', #13137, #17736, #10271 ) ;
#18785 = ORIENTED_EDGE ( 'NONE', *, *, #3867, .F. ) ;
#18786 =( GEOMETRIC_REPRESENTATION_CONTEXT ( 3 ) GLOBAL_UNCERTAINTY_ASSIGNED_CONTEXT ( ( #14722 ) ) GLOBAL_UNIT_ASSIGNED_CONTEXT ( ( #10856, #3483, #16859 ) ) REPRESENTATION_CONTEXT ( 'NONE', 'WORKASPACE' ) );
#18787 = CARTESIAN_POINT ( 'NONE',  ( 8.522092701127531811, 3.777034505568523048, 5.841710761610143798 ) ) ;
#18788 = CARTESIAN_POINT ( 'NONE',  ( 16.56679352167444819, -0.004162264567719712108, -0.008311568981097318051 ) ) ;
#18789 = CARTESIAN_POINT ( 'NONE',  ( 0.3058872367615226295, 10.75034008168916166, 8.562166468153757037 ) ) ;
#18790 = EDGE_LOOP ( 'NONE', ( #10730, #9041, #6497, #8313 ) ) ;
#18791 = FACE_OUTER_BOUND ( 'NONE', #8561, .T. ) ;
#18792 = CARTESIAN_POINT ( 'NONE',  ( -5.000000000000000000, 6.123233995736766282E-16, -3.000000000000000000 ) ) ;
#18793 = CARTESIAN_POINT ( 'NONE',  ( 6.144877202870933530, 7.499999999999866773, -12.52666336607983233 ) ) ;
#18794 = CARTESIAN_POINT ( 'NONE',  ( 1.845755665166725290, -10.33920510797148395, 6.920419570228313333 ) ) ;
#18795 = CARTESIAN_POINT ( 'NONE',  ( -66.35602477868047799, -10.00000000000000888, 3.000000000000000000 ) ) ;
#18796 = CARTESIAN_POINT ( 'NONE',  ( 1.847168016377985333, 4.022276579849959788, 11.77471791462000184 ) ) ;
#18797 = B_SPLINE_CURVE_WITH_KNOTS ( 'NONE', 3,
 ( #12122, #8953, #10690, #14780, #16523, #11922 ),
 .UNSPECIFIED., .F., .F.,
 ( 4, 2, 4 ),
 ( 2.438852479171459636E-18, 0.001657017934711444091, 0.003314035869422886013 ),
 .UNSPECIFIED. ) ;
#18798 = CARTESIAN_POINT ( 'NONE',  ( 2.636624412716062071, -11.10302021258080352, -11.60464335004061454 ) ) ;
#18799 = PRESENTATION_LAYER_ASSIGNMENT (  '', '', ( #12418 ) ) ;
#18800 = B_SPLINE_CURVE_WITH_KNOTS ( 'NONE', 3,
 ( #7939, #2362, #6681, #660, #9534, #13749 ),
 .UNSPECIFIED., .F., .F.,
 ( 4, 2, 4 ),
 ( 9.263427422397552964E-19, 0.001500839035891552656, 0.003001678071783104446 ),
 .UNSPECIFIED. ) ;
#18801 = CARTESIAN_POINT ( 'NONE',  ( -7.000000000000000000, 8.572527594031473190E-16, -12.00000000000000000 ) ) ;
#18802 = VERTEX_POINT ( 'NONE', #736 ) ;
#18803 = ORIENTED_EDGE ( 'NONE', *, *, #3192, .F. ) ;
#18804 = ADVANCED_FACE ( 'NONE', ( #15072 ), #12294, .F. ) ;
#18805 = ADVANCED_FACE ( 'NONE', ( #13737 ), #6477, .T. ) ;
#18806 = EDGE_CURVE ( 'NONE', #14209, #14355, #7193, .T. ) ;
#18807 = EDGE_LOOP ( 'NONE', ( #8766, #6379, #18663, #15899 ) ) ;
#18808 = ORIENTED_EDGE ( 'NONE', *, *, #10540, .F. ) ;
#18809 = ORIENTED_EDGE ( 'NONE', *, *, #13912, .F. ) ;
#18810 = CARTESIAN_POINT ( 'NONE',  ( 2.002547531651519996, 3.242439124566649511, 12.17374746633579541 ) ) ;
#18811 = CARTESIAN_POINT ( 'NONE',  ( -3.335251384444446021, -19.99999999999999645, 6.000000000000000000 ) ) ;
#18812 = DIRECTION ( 'NONE',  ( -0.8629742774544855166, 0.5052478564545411777, -0.000000000000000000 ) ) ;
#18813 = AXIS2_PLACEMENT_3D ( 'NONE', #8603, #14981, #2755 ) ;
#18814 = CARTESIAN_POINT ( 'NONE',  ( 16.56679352167444819, 0.001390132774595458174, 0.009190982326619367287 ) ) ;
#18815 = ORIENTED_EDGE ( 'NONE', *, *, #18872, .F. ) ;
#18816 = CARTESIAN_POINT ( 'NONE',  ( 0.3170788640506440603, 13.02120094575828269, 4.392045232375855868 ) ) ;
#18817 = AXIS2_PLACEMENT_3D ( 'NONE', #1356, #14271, #9852 ) ;
#18818 = LINE ( 'NONE', #16247, #738 ) ;
#18819 = CARTESIAN_POINT ( 'NONE',  ( 0.3137051932979792457, -13.73004976592201842, -0.4596302728641207813 ) ) ;
#18820 = CARTESIAN_POINT ( 'NONE',  ( 0.3151928476913548050, -13.06684726503523919, -4.245457024760359133 ) ) ;
#18821 = CARTESIAN_POINT ( 'NONE',  ( 1.847380140988740926, 11.86779270755359050, 3.740232970470796392 ) ) ;
#18822 = DIRECTION ( 'NONE',  ( 0.000000000000000000, 0.000000000000000000, 1.000000000000000000 ) ) ;
#18823 = AXIS2_PLACEMENT_3D ( 'NONE', #8516, #14341, #1245 ) ;
#18824 = AXIS2_PLACEMENT_3D ( 'NONE', #8084, #3959, #17052 ) ;
#18825 = CARTESIAN_POINT ( 'NONE',  ( 0.000000000000000000, 0.000000000000000000, 0.000000000000000000 ) ) ;
#18826 = CONICAL_SURFACE ( 'NONE', #4808, 8.767949192431130356, 1.308996938995746318 ) ;
#18827 = CARTESIAN_POINT ( 'NONE',  ( 8.522092701127531811, 4.388629235579655230, -5.397361180353095200 ) ) ;
#18828 = ORIENTED_EDGE ( 'NONE', *, *, #11354, .F. ) ;
#18829 = DIRECTION ( 'NONE',  ( 0.000000000000000000, 0.000000000000000000, -1.000000000000000000 ) ) ;
#18831 = ORIENTED_EDGE ( 'NONE', *, *, #849, .T. ) ;
#18830 = CARTESIAN_POINT ( 'NONE',  ( 1.560000000000000053, 0.000000000000000000, 2.999999999999998668 ) ) ;
#18832 = EDGE_CURVE ( 'NONE', #5818, #4766, #6388, .T. ) ;
#18833 = CARTESIAN_POINT ( 'NONE',  ( 0.3142011359265349801, 7.762194356530932815, -11.33549115679415031 ) ) ;
#18834 = ADVANCED_FACE ( 'NONE', ( #9613 ), #2501, .F. ) ;
#18835 = LINE ( 'NONE', #10040, #2205 ) ;
#18836 = ADVANCED_FACE ( 'NONE', ( #3782 ), #10972, .T. ) ;
#18837 =( BOUNDED_SURFACE ( )  B_SPLINE_SURFACE ( 3, 1, ( 
 ( #5344, #11094 ),
 ( #11189, #17182 ),
 ( #9552, #17097 ),
 ( #4001, #2203 ) ),
 .UNSPECIFIED., .F., .F., .T. ) 
 B_SPLINE_SURFACE_WITH_KNOTS ( ( 4, 4 ),
 ( 2, 2 ),
 ( 0.000000000000000000, 1.000000000000000000 ),
 ( 0.000000000000000000, 1.000000000000000000 ),
 .UNSPECIFIED. ) 
 GEOMETRIC_REPRESENTATION_ITEM ( )  RATIONAL_B_SPLINE_SURFACE ( (
 ( 1.000000000000000000, 1.000000000000000000),
 ( 0.7792777138730158093, 0.9689936506012928330),
 ( 0.7792777138730158093, 0.9689936506012928330),
 ( 1.000000000000000000, 1.000000000000000000) ) ) 
 REPRESENTATION_ITEM ( '' )  SURFACE ( )  );
#18838 = VERTEX_POINT ( 'NONE', #10691 ) ;
#18839 = CARTESIAN_POINT ( 'NONE',  ( 3.950837973638676281, -14.41405733518059229, -1.958075594453940971 ) ) ;
#18840 = FACE_OUTER_BOUND ( 'NONE', #10149, .T. ) ;
#18841 = ORIENTED_EDGE ( 'NONE', *, *, #5747, .F. ) ;
#18842 = CARTESIAN_POINT ( 'NONE',  ( 16.56679352167444819, 0.001390132774594440108, -0.009190982326619726375 ) ) ;
#18843 = CARTESIAN_POINT ( 'NONE',  ( 0.3145734862173260038, -4.535879238195024143, 12.96846406299304988 ) ) ;
#18844 = CARTESIAN_POINT ( 'NONE',  ( 0.3148208552358917611, -0.2299193288886511033, -13.73693263646119078 ) ) ;
#18845 = CYLINDRICAL_SURFACE ( 'NONE', #18817, 5.000000000000000000 ) ;
#18846 = VERTEX_POINT ( 'NONE', #10882 ) ;
#18847 = CONTEXT_DEPENDENT_SHAPE_REPRESENTATION ( #13405, #10110 ) ;
#18848 = AXIS2_PLACEMENT_3D ( 'NONE', #5132, #13917, #3312 ) ;
#18849 = DIRECTION ( 'NONE',  ( -1.000000000000000000, -0.000000000000000000, -0.000000000000000000 ) ) ;
#18850 = CARTESIAN_POINT ( 'NONE',  ( -66.35602477868049220, 4.999999999999973355, 5.999999999999999112 ) ) ;
#18851 = CARTESIAN_POINT ( 'NONE',  ( 2.705023505549867924, 12.36217802824812573, -4.909285963183943835 ) ) ;
#18852 = LINE ( 'NONE', #9773, #1654 ) ;
#18853 = CARTESIAN_POINT ( 'NONE',  ( 1.918921323896322750, -12.49850046818174398, -0.6349083173281465653 ) ) ;
#18854 = VERTEX_POINT ( 'NONE', #6571 ) ;
#18855 = FACE_OUTER_BOUND ( 'NONE', #3981, .T. ) ;
#18856 = CARTESIAN_POINT ( 'NONE',  ( 1.560000000000000053, 0.000000000000000000, 0.000000000000000000 ) ) ;
#18857 = ORIENTED_EDGE ( 'NONE', *, *, #7528, .T. ) ;
#18858 = ORIENTED_EDGE ( 'NONE', *, *, #723, .F. ) ;
#18859 = CARTESIAN_POINT ( 'NONE',  ( 2.123976203522053741, -11.67822624909933005, 10.37815841598487765 ) ) ;
#18860 = EDGE_CURVE ( 'NONE', #7279, #1703, #11951, .T. ) ;
#18861 = ORIENTED_EDGE ( 'NONE', *, *, #18614, .F. ) ;
#18862 = CARTESIAN_POINT ( 'NONE',  ( 1.560000000000000053, -1.732050807568877859, -1.752539433813135784E-17 ) ) ;
#18863 = ORIENTED_EDGE ( 'NONE', *, *, #18872, .T. ) ;
#18864 = DIRECTION ( 'NONE',  ( 0.000000000000000000, 0.000000000000000000, 1.000000000000000000 ) ) ;
#18865 = CARTESIAN_POINT ( 'NONE',  ( 1.847168016377985111, -10.17509564929253507, -7.161712042621569019 ) ) ;
#18866 = CARTESIAN_POINT ( 'NONE',  ( 1.846138399168762101, 9.815003036200520725, -7.646096044339786069 ) ) ;
#18868 = CARTESIAN_POINT ( 'NONE',  ( 1.977228804423455610, 11.52787183731216381, -10.21522664410554881 ) ) ;
#18867 =( BOUNDED_SURFACE ( )  B_SPLINE_SURFACE ( 3, 1, ( 
 ( #16107, #2987 ),
 ( #7415, #5964 ),
 ( #14857, #17638 ),
 ( #16198, #6071 ) ),
 .UNSPECIFIED., .F., .F., .T. ) 
 B_SPLINE_SURFACE_WITH_KNOTS ( ( 4, 4 ),
 ( 2, 2 ),
 ( 0.000000000000000000, 1.000000000000000000 ),
 ( 0.000000000000000000, 1.000000000000000000 ),
 .UNSPECIFIED. ) 
 GEOMETRIC_REPRESENTATION_ITEM ( )  RATIONAL_B_SPLINE_SURFACE ( (
 ( 1.000000000000000000, 1.000000000000000000),
 ( 0.9933953342250438912, 0.8357391271907739227),
 ( 0.9933953342250438912, 0.8357391271907739227),
 ( 1.000000000000000000, 1.000000000000000000) ) ) 
 REPRESENTATION_ITEM ( '' )  SURFACE ( )  );
#18869 =( BOUNDED_SURFACE ( )  B_SPLINE_SURFACE ( 3, 1, ( 
 ( #6770, #12580 ),
 ( #6490, #6585 ),
 ( #18144, #5045 ),
 ( #10897, #3795 ) ),
 .UNSPECIFIED., .F., .F., .T. ) 
 B_SPLINE_SURFACE_WITH_KNOTS ( ( 4, 4 ),
 ( 2, 2 ),
 ( 0.000000000000000000, 1.000000000000000000 ),
 ( 0.000000000000000000, 1.000000000000000000 ),
 .UNSPECIFIED. ) 
 GEOMETRIC_REPRESENTATION_ITEM ( )  RATIONAL_B_SPLINE_SURFACE ( (
 ( 1.000000000000000000, 1.000000000000000000),
 ( 0.7792777138730158093, 0.9689936506012928330),
 ( 0.7792777138730158093, 0.9689936506012928330),
 ( 1.000000000000000000, 1.000000000000000000) ) ) 
 REPRESENTATION_ITEM ( '' )  SURFACE ( )  );
#18870 = DIRECTION ( 'NONE',  ( 0.000000000000000000, 0.000000000000000000, 1.000000000000000000 ) ) ;
#18871 = DIRECTION ( 'NONE',  ( -1.000000000000000000, -0.000000000000000000, -0.000000000000000000 ) ) ;
#18872 = EDGE_CURVE ( 'NONE', #11553, #7697, #563, .T. ) ;
#18873 = CARTESIAN_POINT ( 'NONE',  ( 1.562796894703937678, 0.000000000000000000, 0.000000000000000000 ) ) ;
#18874 = CARTESIAN_POINT ( 'NONE',  ( 0.3142014840576500267, 13.73311050063163918, 0.3830336514509360413 ) ) ;
#18875 = ORIENTED_EDGE ( 'NONE', *, *, #18168, .F. ) ;
#18876 = ORIENTED_EDGE ( 'NONE', *, *, #13489, .T. ) ;
#18877 = B_SPLINE_CURVE_WITH_KNOTS ( 'NONE', 3,
 ( #3202, #2087, #18038, #16603 ),
 .UNSPECIFIED., .F., .F.,
 ( 4, 4 ),
 ( 1.140836248210248932E-17, 0.003005512676784841391 ),
 .UNSPECIFIED. ) ;
#18878 = ORIENTED_EDGE ( 'NONE', *, *, #5489, .F. ) ;
#18879 = VERTEX_POINT ( 'NONE', #15175 ) ;
#18880 = VERTEX_POINT ( 'NONE', #16702 ) ;
#18881 = DIRECTION ( 'NONE',  ( -0.000000000000000000, -0.000000000000000000, 1.000000000000000000 ) ) ;
#18882 = FACE_OUTER_BOUND ( 'NONE', #18190, .T. ) ;
#18883 = CARTESIAN_POINT ( 'NONE',  ( 0.3720661004400037664, 10.73619472937702213, 8.694226082900630814 ) ) ;
#18884 = ORIENTED_EDGE ( 'NONE', *, *, #12237, .F. ) ;
#18885 = FACE_OUTER_BOUND ( 'NONE', #745, .T. ) ;
#18886 = ADVANCED_FACE ( 'NONE', ( #13913 ), #3604, .F. ) ;
#18887 = CARTESIAN_POINT ( 'NONE',  ( 3.950837973638675393, 10.05648675950126325, 10.51028938476221342 ) ) ;
#18888 = CARTESIAN_POINT ( 'NONE',  ( 0.4862570985993235340, -7.559321496869339185, -11.67702470553373750 ) ) ;
#18889 = CARTESIAN_POINT ( 'NONE',  ( 2.636624412714292376, 11.60464335004048309, 11.10302021257707850 ) ) ;
#18890 = CARTESIAN_POINT ( 'NONE',  ( 0.3142014840576535795, -11.33546131209467767, 7.762239086932820165 ) ) ;
#18891 = PRESENTATION_LAYER_ASSIGNMENT (  '', '', ( #14315 ) ) ;
#18892 = DIRECTION ( 'NONE',  ( 0.000000000000000000, 0.000000000000000000, 1.000000000000000000 ) ) ;
#18893 = CARTESIAN_POINT ( 'NONE',  ( 1.254009781011619529, -3.563484327698362542, 14.24044713813325558 ) ) ;
#18894 = CARTESIAN_POINT ( 'NONE',  ( 3.950837973638668288, 0.000000000000000000, 0.000000000000000000 ) ) ;
#18895 = CARTESIAN_POINT ( 'NONE',  ( 3.950837973638675393, 2.591948120961804936, 14.31366178983254578 ) ) ;
#18896 = PRESENTATION_LAYER_ASSIGNMENT (  '', '', ( #8236 ) ) ;
#18897 = VERTEX_POINT ( 'NONE', #8464 ) ;
#18898 = ADVANCED_FACE ( 'NONE', ( #7126 ), #5358, .T. ) ;
#18899 =( REPRESENTATION_RELATIONSHIP ('NONE','NONE', #5200, #13515 ) REPRESENTATION_RELATIONSHIP_WITH_TRANSFORMATION ( #4138 )SHAPE_REPRESENTATION_RELATIONSHIP( ) );
#18900 = ORIENTED_EDGE ( 'NONE', *, *, #7986, .T. ) ;
#18901 = EDGE_LOOP ( 'NONE', ( #10935, #18783, #11865, #5393 ) ) ;
#18902 = AXIS2_PLACEMENT_3D ( 'NONE', #6791, #6607, #13857 ) ;
#18903 = VERTEX_POINT ( 'NONE', #1095 ) ;
#18904 = CARTESIAN_POINT ( 'NONE',  ( 1.847380140988739594, 7.402792205949101145, 10.00162556679653214 ) ) ;
#18905 = NEXT_ASSEMBLY_USAGE_OCCURRENCE ( 'NAUO1', ' ', ' ', #6510, #11634, $ ) ;
#18906 = NEXT_ASSEMBLY_USAGE_OCCURRENCE ( 'NAUO2', ' ', ' ', #6510, #3089, $ ) ;
#18907 = NEXT_ASSEMBLY_USAGE_OCCURRENCE ( 'NAUO3', ' ', ' ', #6510, #14430, $ ) ;
#18908 = NEXT_ASSEMBLY_USAGE_OCCURRENCE ( 'NAUO4', ' ', ' ', #6510, #10229, $ ) ;
#18909 = NEXT_ASSEMBLY_USAGE_OCCURRENCE ( 'NAUO5', ' ', ' ', #6510, #12687, $ ) ;
#18910 = NEXT_ASSEMBLY_USAGE_OCCURRENCE ( 'NAUO6', ' ', ' ', #6510, #15021, $ ) ;
#18911 = NEXT_ASSEMBLY_USAGE_OCCURRENCE ( 'NAUO7', ' ', ' ', #6510, #2847, $ ) ;
#18912 = NEXT_ASSEMBLY_USAGE_OCCURRENCE ( 'NAUO8', ' ', ' ', #6510, #1471, $ ) ;
#18913 = NEXT_ASSEMBLY_USAGE_OCCURRENCE ( 'NAUO9', ' ', ' ', #6510, #14430, $ ) ;
#18914 = NEXT_ASSEMBLY_USAGE_OCCURRENCE ( 'NAUO10', ' ', ' ', #6510, #5434, $ ) ;
#18915 = NEXT_ASSEMBLY_USAGE_OCCURRENCE ( 'NAUO11', ' ', ' ', #6510, #2073, $ ) ;
#18916 = NEXT_ASSEMBLY_USAGE_OCCURRENCE ( 'NAUO12', ' ', ' ', #6510, #9645, $ ) ;
#18917 = NEXT_ASSEMBLY_USAGE_OCCURRENCE ( 'NAUO13', ' ', ' ', #6510, #6272, $ ) ;
#18918 = NEXT_ASSEMBLY_USAGE_OCCURRENCE ( 'NAUO14', ' ', ' ', #6510, #16076, $ ) ;
ENDSEC;
END-ISO-10303-21;
